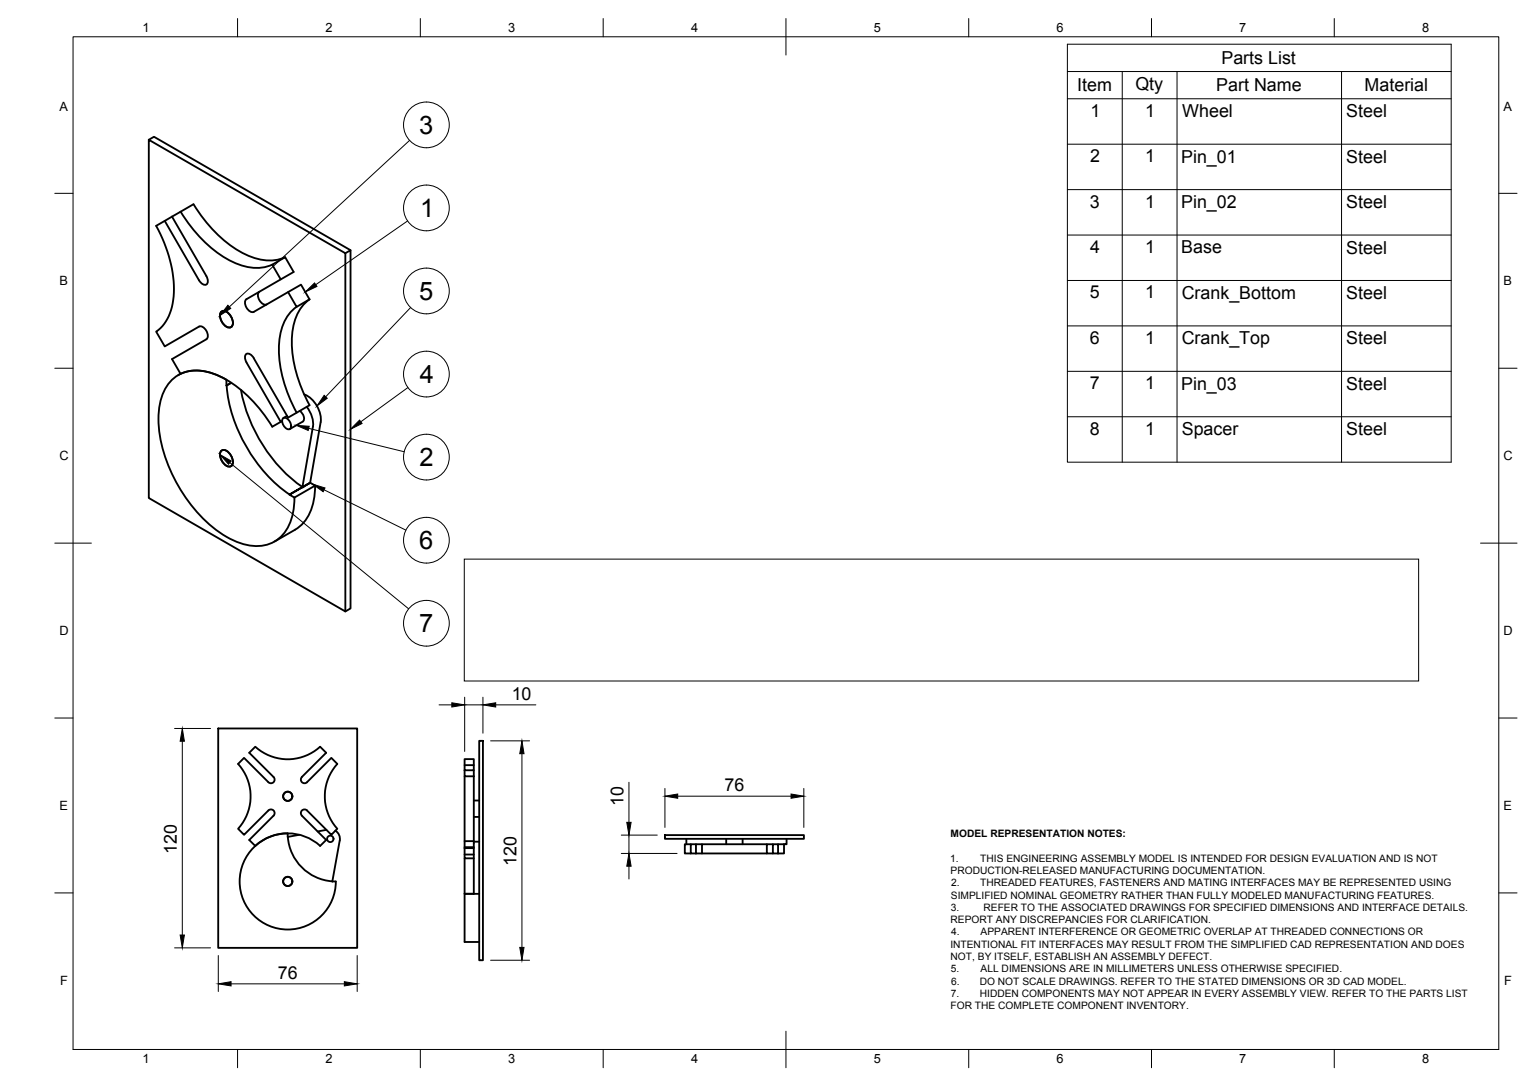
ISO-10303-21;
HEADER;
/* Generated by software containing ST-Developer
 * from STEP Tools, Inc. (www.steptools.com) 
 */

FILE_DESCRIPTION(
/* description */ (''),
/* implementation_level */ '2;1');

FILE_NAME(
/* name */ 'BR-051',
/* time_stamp */ '2026-09-20T21:52:48+06:00',
/* author */ (''),
/* organization */ (''),
/* preprocessor_version */ 'ST-DEVELOPER v20.2',
/* originating_system */ 'Autodesk Translation Framework v15.15.0.0',
/* authorisation */ '');

FILE_SCHEMA (('AUTOMOTIVE_DESIGN { 1 0 10303 214 3 1 1 }'));
ENDSEC;

DATA;
#10=MECHANICAL_DESIGN_GEOMETRIC_PRESENTATION_REPRESENTATION('',(#59,#60,
#61,#62,#63,#64,#65,#66),#2203);
#11=ITEM_DEFINED_TRANSFORMATION($,$,#1324,#1449);
#12=ITEM_DEFINED_TRANSFORMATION($,$,#1370,#1450);
#13=ITEM_DEFINED_TRANSFORMATION($,$,#1376,#1451);
#14=ITEM_DEFINED_TRANSFORMATION($,$,#1382,#1452);
#15=ITEM_DEFINED_TRANSFORMATION($,$,#1395,#1453);
#16=ITEM_DEFINED_TRANSFORMATION($,$,#1414,#1454);
#17=ITEM_DEFINED_TRANSFORMATION($,$,#1434,#1455);
#18=ITEM_DEFINED_TRANSFORMATION($,$,#1440,#1456);
#19=(
REPRESENTATION_RELATIONSHIP($,$,#2235,#2234)
REPRESENTATION_RELATIONSHIP_WITH_TRANSFORMATION(#11)
SHAPE_REPRESENTATION_RELATIONSHIP()
);
#20=(
REPRESENTATION_RELATIONSHIP($,$,#2236,#2234)
REPRESENTATION_RELATIONSHIP_WITH_TRANSFORMATION(#12)
SHAPE_REPRESENTATION_RELATIONSHIP()
);
#21=(
REPRESENTATION_RELATIONSHIP($,$,#2237,#2234)
REPRESENTATION_RELATIONSHIP_WITH_TRANSFORMATION(#13)
SHAPE_REPRESENTATION_RELATIONSHIP()
);
#22=(
REPRESENTATION_RELATIONSHIP($,$,#2238,#2234)
REPRESENTATION_RELATIONSHIP_WITH_TRANSFORMATION(#14)
SHAPE_REPRESENTATION_RELATIONSHIP()
);
#23=(
REPRESENTATION_RELATIONSHIP($,$,#2239,#2234)
REPRESENTATION_RELATIONSHIP_WITH_TRANSFORMATION(#15)
SHAPE_REPRESENTATION_RELATIONSHIP()
);
#24=(
REPRESENTATION_RELATIONSHIP($,$,#2240,#2234)
REPRESENTATION_RELATIONSHIP_WITH_TRANSFORMATION(#16)
SHAPE_REPRESENTATION_RELATIONSHIP()
);
#25=(
REPRESENTATION_RELATIONSHIP($,$,#2241,#2234)
REPRESENTATION_RELATIONSHIP_WITH_TRANSFORMATION(#17)
SHAPE_REPRESENTATION_RELATIONSHIP()
);
#26=(
REPRESENTATION_RELATIONSHIP($,$,#2242,#2234)
REPRESENTATION_RELATIONSHIP_WITH_TRANSFORMATION(#18)
SHAPE_REPRESENTATION_RELATIONSHIP()
);
#27=CONTEXT_DEPENDENT_SHAPE_REPRESENTATION(#19,#2226);
#28=CONTEXT_DEPENDENT_SHAPE_REPRESENTATION(#20,#2227);
#29=CONTEXT_DEPENDENT_SHAPE_REPRESENTATION(#21,#2228);
#30=CONTEXT_DEPENDENT_SHAPE_REPRESENTATION(#22,#2229);
#31=CONTEXT_DEPENDENT_SHAPE_REPRESENTATION(#23,#2230);
#32=CONTEXT_DEPENDENT_SHAPE_REPRESENTATION(#24,#2231);
#33=CONTEXT_DEPENDENT_SHAPE_REPRESENTATION(#25,#2232);
#34=CONTEXT_DEPENDENT_SHAPE_REPRESENTATION(#26,#2233);
#35=NEXT_ASSEMBLY_USAGE_OCCURRENCE('Wheel:1','Wheel:1','Wheel:1',#2244,
#2245,'Wheel:1');
#36=NEXT_ASSEMBLY_USAGE_OCCURRENCE('Pin_01:1','Pin_01:1','Pin_01:1',#2244,
#2246,'Pin_01:1');
#37=NEXT_ASSEMBLY_USAGE_OCCURRENCE('Pin_02:1','Pin_02:1','Pin_02:1',#2244,
#2247,'Pin_02:1');
#38=NEXT_ASSEMBLY_USAGE_OCCURRENCE('Base:1','Base:1','Base:1',#2244,#2248,
'Base:1');
#39=NEXT_ASSEMBLY_USAGE_OCCURRENCE('Crank_Bottom:1','Crank_Bottom:1',
'Crank_Bottom:1',#2244,#2249,'Crank_Bottom:1');
#40=NEXT_ASSEMBLY_USAGE_OCCURRENCE('Crank_Top:1','Crank_Top:1',
'Crank_Top:1',#2244,#2250,'Crank_Top:1');
#41=NEXT_ASSEMBLY_USAGE_OCCURRENCE('Pin_03:1','Pin_03:1','Pin_03:1',#2244,
#2251,'Pin_03:1');
#42=NEXT_ASSEMBLY_USAGE_OCCURRENCE('Spacer:1','Spacer:1','Spacer:1',#2244,
#2252,'Spacer:1');
#43=SHAPE_REPRESENTATION_RELATIONSHIP('SRR','None',#2235,#51);
#44=SHAPE_REPRESENTATION_RELATIONSHIP('SRR','None',#2236,#52);
#45=SHAPE_REPRESENTATION_RELATIONSHIP('SRR','None',#2237,#53);
#46=SHAPE_REPRESENTATION_RELATIONSHIP('SRR','None',#2238,#54);
#47=SHAPE_REPRESENTATION_RELATIONSHIP('SRR','None',#2239,#55);
#48=SHAPE_REPRESENTATION_RELATIONSHIP('SRR','None',#2240,#56);
#49=SHAPE_REPRESENTATION_RELATIONSHIP('SRR','None',#2241,#57);
#50=SHAPE_REPRESENTATION_RELATIONSHIP('SRR','None',#2242,#58);
#51=ADVANCED_BREP_SHAPE_REPRESENTATION('',(#67),#2195);
#52=ADVANCED_BREP_SHAPE_REPRESENTATION('',(#68),#2196);
#53=ADVANCED_BREP_SHAPE_REPRESENTATION('',(#69),#2197);
#54=ADVANCED_BREP_SHAPE_REPRESENTATION('',(#70),#2198);
#55=ADVANCED_BREP_SHAPE_REPRESENTATION('',(#71),#2199);
#56=ADVANCED_BREP_SHAPE_REPRESENTATION('',(#72),#2200);
#57=ADVANCED_BREP_SHAPE_REPRESENTATION('',(#73),#2201);
#58=ADVANCED_BREP_SHAPE_REPRESENTATION('',(#74),#2202);
#59=STYLED_ITEM('',(#2284),#67);
#60=STYLED_ITEM('',(#2285),#68);
#61=STYLED_ITEM('',(#2286),#69);
#62=STYLED_ITEM('',(#2286),#70);
#63=STYLED_ITEM('',(#2285),#71);
#64=STYLED_ITEM('',(#2285),#72);
#65=STYLED_ITEM('',(#2286),#73);
#66=STYLED_ITEM('',(#2286),#74);
#67=MANIFOLD_SOLID_BREP('Wheel',#1226);
#68=MANIFOLD_SOLID_BREP('Pin_01',#1227);
#69=MANIFOLD_SOLID_BREP('Pin_02',#1228);
#70=MANIFOLD_SOLID_BREP('Base',#1229);
#71=MANIFOLD_SOLID_BREP('Crank_Bottom',#1230);
#72=MANIFOLD_SOLID_BREP('Crank_Top',#1231);
#73=MANIFOLD_SOLID_BREP('Pin_03',#1232);
#74=MANIFOLD_SOLID_BREP('Spacer',#1233);
#75=FACE_BOUND('',#256,.T.);
#76=FACE_BOUND('',#258,.T.);
#77=FACE_BOUND('',#268,.T.);
#78=FACE_BOUND('',#269,.T.);
#79=FACE_BOUND('',#275,.T.);
#80=FACE_BOUND('',#276,.T.);
#81=FACE_BOUND('',#280,.T.);
#82=FACE_BOUND('',#281,.T.);
#83=FACE_BOUND('',#288,.T.);
#84=FACE_BOUND('',#289,.T.);
#85=FACE_BOUND('',#297,.T.);
#86=FACE_BOUND('',#303,.T.);
#87=FACE_BOUND('',#308,.T.);
#88=FACE_BOUND('',#312,.T.);
#89=CIRCLE('',#1327,2.);
#90=CIRCLE('',#1328,2.);
#91=CIRCLE('',#1334,2.);
#92=CIRCLE('',#1335,2.);
#93=CIRCLE('',#1339,26.3);
#94=CIRCLE('',#1340,26.3);
#95=CIRCLE('',#1344,2.);
#96=CIRCLE('',#1345,2.);
#97=CIRCLE('',#1349,26.3);
#98=CIRCLE('',#1350,26.3);
#99=CIRCLE('',#1354,2.);
#100=CIRCLE('',#1355,2.);
#101=CIRCLE('',#1359,26.3);
#102=CIRCLE('',#1360,26.3);
#103=CIRCLE('',#1362,2.5);
#104=CIRCLE('',#1363,2.5);
#105=CIRCLE('',#1365,26.3);
#106=CIRCLE('',#1366,26.3);
#107=CIRCLE('',#1372,1.75);
#108=CIRCLE('',#1374,1.75);
#109=CIRCLE('',#1378,2.5);
#110=CIRCLE('',#1380,2.5);
#111=CIRCLE('',#1384,2.5);
#112=CIRCLE('',#1385,2.5);
#113=CIRCLE('',#1387,2.5);
#114=CIRCLE('',#1388,2.5);
#115=CIRCLE('',#1399,5.25);
#116=CIRCLE('',#1400,24.399223777829);
#117=CIRCLE('',#1401,2.5);
#118=CIRCLE('',#1402,1.75);
#119=CIRCLE('',#1405,5.25);
#120=CIRCLE('',#1407,1.75);
#121=CIRCLE('',#1410,2.5);
#122=CIRCLE('',#1412,24.399223777829);
#123=CIRCLE('',#1417,24.399223777829);
#124=CIRCLE('',#1418,26.3);
#125=CIRCLE('',#1420,24.399223777829);
#126=CIRCLE('',#1422,26.3);
#127=CIRCLE('',#1425,26.3);
#128=CIRCLE('',#1426,2.5);
#129=CIRCLE('',#1428,26.3);
#130=CIRCLE('',#1430,2.5);
#131=CIRCLE('',#1436,2.5);
#132=CIRCLE('',#1438,2.5);
#133=CIRCLE('',#1442,4.5);
#134=CIRCLE('',#1443,2.5);
#135=CIRCLE('',#1445,4.5);
#136=CIRCLE('',#1447,2.5);
#137=CYLINDRICAL_SURFACE('',#1326,2.);
#138=CYLINDRICAL_SURFACE('',#1333,2.);
#139=CYLINDRICAL_SURFACE('',#1338,26.3);
#140=CYLINDRICAL_SURFACE('',#1343,2.);
#141=CYLINDRICAL_SURFACE('',#1348,26.3);
#142=CYLINDRICAL_SURFACE('',#1353,2.);
#143=CYLINDRICAL_SURFACE('',#1358,26.3);
#144=CYLINDRICAL_SURFACE('',#1361,2.5);
#145=CYLINDRICAL_SURFACE('',#1364,26.3);
#146=CYLINDRICAL_SURFACE('',#1373,1.75);
#147=CYLINDRICAL_SURFACE('',#1379,2.5);
#148=CYLINDRICAL_SURFACE('',#1383,2.5);
#149=CYLINDRICAL_SURFACE('',#1386,2.5);
#150=CYLINDRICAL_SURFACE('',#1404,5.25);
#151=CYLINDRICAL_SURFACE('',#1406,1.75);
#152=CYLINDRICAL_SURFACE('',#1409,2.5);
#153=CYLINDRICAL_SURFACE('',#1413,24.399223777829);
#154=CYLINDRICAL_SURFACE('',#1419,24.399223777829);
#155=CYLINDRICAL_SURFACE('',#1421,26.3);
#156=CYLINDRICAL_SURFACE('',#1427,26.3);
#157=CYLINDRICAL_SURFACE('',#1429,2.5);
#158=CYLINDRICAL_SURFACE('',#1437,2.5);
#159=CYLINDRICAL_SURFACE('',#1444,4.5);
#160=CYLINDRICAL_SURFACE('',#1446,2.5);
#161=FACE_OUTER_BOUND('',#230,.T.);
#162=FACE_OUTER_BOUND('',#231,.T.);
#163=FACE_OUTER_BOUND('',#232,.T.);
#164=FACE_OUTER_BOUND('',#233,.T.);
#165=FACE_OUTER_BOUND('',#234,.T.);
#166=FACE_OUTER_BOUND('',#235,.T.);
#167=FACE_OUTER_BOUND('',#236,.T.);
#168=FACE_OUTER_BOUND('',#237,.T.);
#169=FACE_OUTER_BOUND('',#238,.T.);
#170=FACE_OUTER_BOUND('',#239,.T.);
#171=FACE_OUTER_BOUND('',#240,.T.);
#172=FACE_OUTER_BOUND('',#241,.T.);
#173=FACE_OUTER_BOUND('',#242,.T.);
#174=FACE_OUTER_BOUND('',#243,.T.);
#175=FACE_OUTER_BOUND('',#244,.T.);
#176=FACE_OUTER_BOUND('',#245,.T.);
#177=FACE_OUTER_BOUND('',#246,.T.);
#178=FACE_OUTER_BOUND('',#247,.T.);
#179=FACE_OUTER_BOUND('',#248,.T.);
#180=FACE_OUTER_BOUND('',#249,.T.);
#181=FACE_OUTER_BOUND('',#250,.T.);
#182=FACE_OUTER_BOUND('',#251,.T.);
#183=FACE_OUTER_BOUND('',#252,.T.);
#184=FACE_OUTER_BOUND('',#253,.T.);
#185=FACE_OUTER_BOUND('',#254,.T.);
#186=FACE_OUTER_BOUND('',#255,.T.);
#187=FACE_OUTER_BOUND('',#257,.T.);
#188=FACE_OUTER_BOUND('',#259,.T.);
#189=FACE_OUTER_BOUND('',#260,.T.);
#190=FACE_OUTER_BOUND('',#261,.T.);
#191=FACE_OUTER_BOUND('',#262,.T.);
#192=FACE_OUTER_BOUND('',#263,.T.);
#193=FACE_OUTER_BOUND('',#264,.T.);
#194=FACE_OUTER_BOUND('',#265,.T.);
#195=FACE_OUTER_BOUND('',#266,.T.);
#196=FACE_OUTER_BOUND('',#267,.T.);
#197=FACE_OUTER_BOUND('',#270,.T.);
#198=FACE_OUTER_BOUND('',#271,.T.);
#199=FACE_OUTER_BOUND('',#272,.T.);
#200=FACE_OUTER_BOUND('',#273,.T.);
#201=FACE_OUTER_BOUND('',#274,.T.);
#202=FACE_OUTER_BOUND('',#277,.T.);
#203=FACE_OUTER_BOUND('',#278,.T.);
#204=FACE_OUTER_BOUND('',#279,.T.);
#205=FACE_OUTER_BOUND('',#282,.T.);
#206=FACE_OUTER_BOUND('',#283,.T.);
#207=FACE_OUTER_BOUND('',#284,.T.);
#208=FACE_OUTER_BOUND('',#285,.T.);
#209=FACE_OUTER_BOUND('',#286,.T.);
#210=FACE_OUTER_BOUND('',#287,.T.);
#211=FACE_OUTER_BOUND('',#290,.T.);
#212=FACE_OUTER_BOUND('',#291,.T.);
#213=FACE_OUTER_BOUND('',#292,.T.);
#214=FACE_OUTER_BOUND('',#293,.T.);
#215=FACE_OUTER_BOUND('',#294,.T.);
#216=FACE_OUTER_BOUND('',#295,.T.);
#217=FACE_OUTER_BOUND('',#296,.T.);
#218=FACE_OUTER_BOUND('',#298,.T.);
#219=FACE_OUTER_BOUND('',#299,.T.);
#220=FACE_OUTER_BOUND('',#300,.T.);
#221=FACE_OUTER_BOUND('',#301,.T.);
#222=FACE_OUTER_BOUND('',#302,.T.);
#223=FACE_OUTER_BOUND('',#304,.T.);
#224=FACE_OUTER_BOUND('',#305,.T.);
#225=FACE_OUTER_BOUND('',#306,.T.);
#226=FACE_OUTER_BOUND('',#307,.T.);
#227=FACE_OUTER_BOUND('',#309,.T.);
#228=FACE_OUTER_BOUND('',#310,.T.);
#229=FACE_OUTER_BOUND('',#311,.T.);
#230=EDGE_LOOP('',(#796,#797,#798,#799));
#231=EDGE_LOOP('',(#800,#801,#802,#803));
#232=EDGE_LOOP('',(#804,#805,#806,#807));
#233=EDGE_LOOP('',(#808,#809,#810,#811));
#234=EDGE_LOOP('',(#812,#813,#814,#815));
#235=EDGE_LOOP('',(#816,#817,#818,#819));
#236=EDGE_LOOP('',(#820,#821,#822,#823));
#237=EDGE_LOOP('',(#824,#825,#826,#827));
#238=EDGE_LOOP('',(#828,#829,#830,#831));
#239=EDGE_LOOP('',(#832,#833,#834,#835));
#240=EDGE_LOOP('',(#836,#837,#838,#839));
#241=EDGE_LOOP('',(#840,#841,#842,#843));
#242=EDGE_LOOP('',(#844,#845,#846,#847));
#243=EDGE_LOOP('',(#848,#849,#850,#851));
#244=EDGE_LOOP('',(#852,#853,#854,#855));
#245=EDGE_LOOP('',(#856,#857,#858,#859));
#246=EDGE_LOOP('',(#860,#861,#862,#863));
#247=EDGE_LOOP('',(#864,#865,#866,#867));
#248=EDGE_LOOP('',(#868,#869,#870,#871));
#249=EDGE_LOOP('',(#872,#873,#874,#875));
#250=EDGE_LOOP('',(#876,#877,#878,#879));
#251=EDGE_LOOP('',(#880,#881,#882,#883));
#252=EDGE_LOOP('',(#884,#885,#886,#887));
#253=EDGE_LOOP('',(#888,#889,#890,#891));
#254=EDGE_LOOP('',(#892,#893,#894,#895));
#255=EDGE_LOOP('',(#896,#897,#898,#899,#900,#901,#902,#903,#904,#905,#906,
#907,#908,#909,#910,#911,#912,#913,#914,#915,#916,#917,#918,#919));
#256=EDGE_LOOP('',(#920));
#257=EDGE_LOOP('',(#921,#922,#923,#924,#925,#926,#927,#928,#929,#930,#931,
#932,#933,#934,#935,#936,#937,#938,#939,#940,#941,#942,#943,#944));
#258=EDGE_LOOP('',(#945));
#259=EDGE_LOOP('',(#946));
#260=EDGE_LOOP('',(#947,#948,#949,#950));
#261=EDGE_LOOP('',(#951));
#262=EDGE_LOOP('',(#952));
#263=EDGE_LOOP('',(#953,#954,#955,#956));
#264=EDGE_LOOP('',(#957));
#265=EDGE_LOOP('',(#958,#959,#960,#961));
#266=EDGE_LOOP('',(#962,#963,#964,#965));
#267=EDGE_LOOP('',(#966,#967,#968,#969));
#268=EDGE_LOOP('',(#970));
#269=EDGE_LOOP('',(#971));
#270=EDGE_LOOP('',(#972,#973,#974,#975));
#271=EDGE_LOOP('',(#976,#977,#978,#979));
#272=EDGE_LOOP('',(#980,#981,#982,#983));
#273=EDGE_LOOP('',(#984,#985,#986,#987));
#274=EDGE_LOOP('',(#988,#989,#990,#991));
#275=EDGE_LOOP('',(#992));
#276=EDGE_LOOP('',(#993));
#277=EDGE_LOOP('',(#994,#995,#996,#997));
#278=EDGE_LOOP('',(#998,#999,#1000,#1001));
#279=EDGE_LOOP('',(#1002,#1003,#1004,#1005,#1006,#1007));
#280=EDGE_LOOP('',(#1008));
#281=EDGE_LOOP('',(#1009));
#282=EDGE_LOOP('',(#1010,#1011,#1012,#1013));
#283=EDGE_LOOP('',(#1014,#1015,#1016,#1017));
#284=EDGE_LOOP('',(#1018,#1019,#1020,#1021));
#285=EDGE_LOOP('',(#1022,#1023,#1024,#1025));
#286=EDGE_LOOP('',(#1026,#1027,#1028,#1029));
#287=EDGE_LOOP('',(#1030,#1031,#1032,#1033,#1034,#1035));
#288=EDGE_LOOP('',(#1036));
#289=EDGE_LOOP('',(#1037));
#290=EDGE_LOOP('',(#1038,#1039,#1040,#1041));
#291=EDGE_LOOP('',(#1042,#1043,#1044,#1045,#1046));
#292=EDGE_LOOP('',(#1047,#1048,#1049,#1050));
#293=EDGE_LOOP('',(#1051,#1052,#1053,#1054));
#294=EDGE_LOOP('',(#1055,#1056,#1057,#1058));
#295=EDGE_LOOP('',(#1059,#1060,#1061,#1062));
#296=EDGE_LOOP('',(#1063,#1064,#1065,#1066,#1067,#1068));
#297=EDGE_LOOP('',(#1069));
#298=EDGE_LOOP('',(#1070,#1071,#1072,#1073));
#299=EDGE_LOOP('',(#1074,#1075,#1076,#1077));
#300=EDGE_LOOP('',(#1078,#1079,#1080,#1081,#1082,#1083));
#301=EDGE_LOOP('',(#1084,#1085,#1086,#1087));
#302=EDGE_LOOP('',(#1088,#1089,#1090,#1091,#1092));
#303=EDGE_LOOP('',(#1093));
#304=EDGE_LOOP('',(#1094));
#305=EDGE_LOOP('',(#1095,#1096,#1097,#1098));
#306=EDGE_LOOP('',(#1099));
#307=EDGE_LOOP('',(#1100));
#308=EDGE_LOOP('',(#1101));
#309=EDGE_LOOP('',(#1102,#1103,#1104,#1105));
#310=EDGE_LOOP('',(#1106,#1107,#1108,#1109));
#311=EDGE_LOOP('',(#1110));
#312=EDGE_LOOP('',(#1111));
#313=LINE('',#1840,#423);
#314=LINE('',#1842,#424);
#315=LINE('',#1844,#425);
#316=LINE('',#1845,#426);
#317=LINE('',#1851,#427);
#318=LINE('',#1854,#428);
#319=LINE('',#1856,#429);
#320=LINE('',#1857,#430);
#321=LINE('',#1860,#431);
#322=LINE('',#1862,#432);
#323=LINE('',#1863,#433);
#324=LINE('',#1866,#434);
#325=LINE('',#1868,#435);
#326=LINE('',#1869,#436);
#327=LINE('',#1873,#437);
#328=LINE('',#1875,#438);
#329=LINE('',#1877,#439);
#330=LINE('',#1878,#440);
#331=LINE('',#1883,#441);
#332=LINE('',#1887,#442);
#333=LINE('',#1889,#443);
#334=LINE('',#1890,#444);
#335=LINE('',#1893,#445);
#336=LINE('',#1895,#446);
#337=LINE('',#1896,#447);
#338=LINE('',#1902,#448);
#339=LINE('',#1904,#449);
#340=LINE('',#1905,#450);
#341=LINE('',#1909,#451);
#342=LINE('',#1911,#452);
#343=LINE('',#1913,#453);
#344=LINE('',#1914,#454);
#345=LINE('',#1919,#455);
#346=LINE('',#1923,#456);
#347=LINE('',#1925,#457);
#348=LINE('',#1926,#458);
#349=LINE('',#1929,#459);
#350=LINE('',#1931,#460);
#351=LINE('',#1932,#461);
#352=LINE('',#1937,#462);
#353=LINE('',#1940,#463);
#354=LINE('',#1941,#464);
#355=LINE('',#1945,#465);
#356=LINE('',#1947,#466);
#357=LINE('',#1949,#467);
#358=LINE('',#1950,#468);
#359=LINE('',#1956,#469);
#360=LINE('',#1959,#470);
#361=LINE('',#1961,#471);
#362=LINE('',#1962,#472);
#363=LINE('',#1965,#473);
#364=LINE('',#1967,#474);
#365=LINE('',#1968,#475);
#366=LINE('',#1976,#476);
#367=LINE('',#1983,#477);
#368=LINE('',#1985,#478);
#369=LINE('',#1986,#479);
#370=LINE('',#1995,#480);
#371=LINE('',#2004,#481);
#372=LINE('',#2012,#482);
#373=LINE('',#2018,#483);
#374=LINE('',#2023,#484);
#375=LINE('',#2025,#485);
#376=LINE('',#2027,#486);
#377=LINE('',#2028,#487);
#378=LINE('',#2031,#488);
#379=LINE('',#2033,#489);
#380=LINE('',#2034,#490);
#381=LINE('',#2037,#491);
#382=LINE('',#2038,#492);
#383=LINE('',#2041,#493);
#384=LINE('',#2042,#494);
#385=LINE('',#2044,#495);
#386=LINE('',#2050,#496);
#387=LINE('',#2052,#497);
#388=LINE('',#2054,#498);
#389=LINE('',#2055,#499);
#390=LINE('',#2059,#500);
#391=LINE('',#2061,#501);
#392=LINE('',#2063,#502);
#393=LINE('',#2064,#503);
#394=LINE('',#2067,#504);
#395=LINE('',#2070,#505);
#396=LINE('',#2078,#506);
#397=LINE('',#2079,#507);
#398=LINE('',#2084,#508);
#399=LINE('',#2088,#509);
#400=LINE('',#2089,#510);
#401=LINE('',#2092,#511);
#402=LINE('',#2101,#512);
#403=LINE('',#2103,#513);
#404=LINE('',#2105,#514);
#405=LINE('',#2107,#515);
#406=LINE('',#2108,#516);
#407=LINE('',#2113,#517);
#408=LINE('',#2118,#518);
#409=LINE('',#2121,#519);
#410=LINE('',#2126,#520);
#411=LINE('',#2128,#521);
#412=LINE('',#2130,#522);
#413=LINE('',#2131,#523);
#414=LINE('',#2134,#524);
#415=LINE('',#2135,#525);
#416=LINE('',#2141,#526);
#417=LINE('',#2146,#527);
#418=LINE('',#2148,#528);
#419=LINE('',#2150,#529);
#420=LINE('',#2158,#530);
#421=LINE('',#2169,#531);
#422=LINE('',#2174,#532);
#423=VECTOR('',#1463,10.);
#424=VECTOR('',#1464,10.);
#425=VECTOR('',#1465,10.);
#426=VECTOR('',#1466,10.);
#427=VECTOR('',#1473,10.);
#428=VECTOR('',#1476,10.);
#429=VECTOR('',#1477,10.);
#430=VECTOR('',#1478,10.);
#431=VECTOR('',#1481,10.);
#432=VECTOR('',#1482,10.);
#433=VECTOR('',#1483,10.);
#434=VECTOR('',#1486,10.);
#435=VECTOR('',#1487,10.);
#436=VECTOR('',#1488,10.);
#437=VECTOR('',#1491,10.);
#438=VECTOR('',#1492,10.);
#439=VECTOR('',#1493,10.);
#440=VECTOR('',#1494,10.);
#441=VECTOR('',#1499,10.);
#442=VECTOR('',#1504,10.);
#443=VECTOR('',#1505,10.);
#444=VECTOR('',#1506,10.);
#445=VECTOR('',#1509,10.);
#446=VECTOR('',#1510,10.);
#447=VECTOR('',#1511,10.);
#448=VECTOR('',#1520,10.);
#449=VECTOR('',#1521,10.);
#450=VECTOR('',#1522,10.);
#451=VECTOR('',#1525,10.);
#452=VECTOR('',#1526,10.);
#453=VECTOR('',#1527,10.);
#454=VECTOR('',#1528,10.);
#455=VECTOR('',#1533,10.);
#456=VECTOR('',#1538,10.);
#457=VECTOR('',#1539,10.);
#458=VECTOR('',#1540,10.);
#459=VECTOR('',#1543,10.);
#460=VECTOR('',#1544,10.);
#461=VECTOR('',#1545,10.);
#462=VECTOR('',#1550,10.);
#463=VECTOR('',#1555,10.);
#464=VECTOR('',#1556,10.);
#465=VECTOR('',#1559,10.);
#466=VECTOR('',#1560,10.);
#467=VECTOR('',#1561,10.);
#468=VECTOR('',#1562,10.);
#469=VECTOR('',#1569,10.);
#470=VECTOR('',#1572,10.);
#471=VECTOR('',#1573,10.);
#472=VECTOR('',#1574,10.);
#473=VECTOR('',#1577,10.);
#474=VECTOR('',#1578,10.);
#475=VECTOR('',#1579,10.);
#476=VECTOR('',#1590,2.5);
#477=VECTOR('',#1599,10.);
#478=VECTOR('',#1602,10.);
#479=VECTOR('',#1603,10.);
#480=VECTOR('',#1616,1.75);
#481=VECTOR('',#1629,2.5);
#482=VECTOR('',#1640,2.5);
#483=VECTOR('',#1647,2.5);
#484=VECTOR('',#1652,10.);
#485=VECTOR('',#1653,10.);
#486=VECTOR('',#1654,10.);
#487=VECTOR('',#1655,10.);
#488=VECTOR('',#1658,10.);
#489=VECTOR('',#1659,10.);
#490=VECTOR('',#1660,10.);
#491=VECTOR('',#1663,10.);
#492=VECTOR('',#1664,10.);
#493=VECTOR('',#1667,10.);
#494=VECTOR('',#1668,10.);
#495=VECTOR('',#1671,10.);
#496=VECTOR('',#1678,10.);
#497=VECTOR('',#1679,10.);
#498=VECTOR('',#1680,10.);
#499=VECTOR('',#1681,10.);
#500=VECTOR('',#1684,10.);
#501=VECTOR('',#1685,10.);
#502=VECTOR('',#1686,10.);
#503=VECTOR('',#1687,10.);
#504=VECTOR('',#1690,10.);
#505=VECTOR('',#1693,10.);
#506=VECTOR('',#1702,10.);
#507=VECTOR('',#1703,10.);
#508=VECTOR('',#1710,1.75);
#509=VECTOR('',#1715,10.);
#510=VECTOR('',#1716,10.);
#511=VECTOR('',#1719,2.5);
#512=VECTOR('',#1732,10.);
#513=VECTOR('',#1733,10.);
#514=VECTOR('',#1734,10.);
#515=VECTOR('',#1735,10.);
#516=VECTOR('',#1736,10.);
#517=VECTOR('',#1741,10.);
#518=VECTOR('',#1748,10.);
#519=VECTOR('',#1751,10.);
#520=VECTOR('',#1756,10.);
#521=VECTOR('',#1757,10.);
#522=VECTOR('',#1758,10.);
#523=VECTOR('',#1759,10.);
#524=VECTOR('',#1762,10.);
#525=VECTOR('',#1763,10.);
#526=VECTOR('',#1770,10.);
#527=VECTOR('',#1777,2.5);
#528=VECTOR('',#1780,10.);
#529=VECTOR('',#1783,10.);
#530=VECTOR('',#1794,2.5);
#531=VECTOR('',#1809,4.5);
#532=VECTOR('',#1816,2.5);
#533=VERTEX_POINT('',#1838);
#534=VERTEX_POINT('',#1839);
#535=VERTEX_POINT('',#1841);
#536=VERTEX_POINT('',#1843);
#537=VERTEX_POINT('',#1847);
#538=VERTEX_POINT('',#1849);
#539=VERTEX_POINT('',#1853);
#540=VERTEX_POINT('',#1855);
#541=VERTEX_POINT('',#1859);
#542=VERTEX_POINT('',#1861);
#543=VERTEX_POINT('',#1865);
#544=VERTEX_POINT('',#1867);
#545=VERTEX_POINT('',#1871);
#546=VERTEX_POINT('',#1872);
#547=VERTEX_POINT('',#1874);
#548=VERTEX_POINT('',#1876);
#549=VERTEX_POINT('',#1880);
#550=VERTEX_POINT('',#1882);
#551=VERTEX_POINT('',#1886);
#552=VERTEX_POINT('',#1888);
#553=VERTEX_POINT('',#1892);
#554=VERTEX_POINT('',#1894);
#555=VERTEX_POINT('',#1901);
#556=VERTEX_POINT('',#1903);
#557=VERTEX_POINT('',#1907);
#558=VERTEX_POINT('',#1908);
#559=VERTEX_POINT('',#1910);
#560=VERTEX_POINT('',#1912);
#561=VERTEX_POINT('',#1916);
#562=VERTEX_POINT('',#1918);
#563=VERTEX_POINT('',#1922);
#564=VERTEX_POINT('',#1924);
#565=VERTEX_POINT('',#1928);
#566=VERTEX_POINT('',#1930);
#567=VERTEX_POINT('',#1934);
#568=VERTEX_POINT('',#1936);
#569=VERTEX_POINT('',#1943);
#570=VERTEX_POINT('',#1944);
#571=VERTEX_POINT('',#1946);
#572=VERTEX_POINT('',#1948);
#573=VERTEX_POINT('',#1952);
#574=VERTEX_POINT('',#1954);
#575=VERTEX_POINT('',#1958);
#576=VERTEX_POINT('',#1960);
#577=VERTEX_POINT('',#1964);
#578=VERTEX_POINT('',#1966);
#579=VERTEX_POINT('',#1973);
#580=VERTEX_POINT('',#1975);
#581=VERTEX_POINT('',#1979);
#582=VERTEX_POINT('',#1981);
#583=VERTEX_POINT('',#1991);
#584=VERTEX_POINT('',#1994);
#585=VERTEX_POINT('',#2000);
#586=VERTEX_POINT('',#2003);
#587=VERTEX_POINT('',#2009);
#588=VERTEX_POINT('',#2011);
#589=VERTEX_POINT('',#2015);
#590=VERTEX_POINT('',#2017);
#591=VERTEX_POINT('',#2021);
#592=VERTEX_POINT('',#2022);
#593=VERTEX_POINT('',#2024);
#594=VERTEX_POINT('',#2026);
#595=VERTEX_POINT('',#2030);
#596=VERTEX_POINT('',#2032);
#597=VERTEX_POINT('',#2036);
#598=VERTEX_POINT('',#2040);
#599=VERTEX_POINT('',#2048);
#600=VERTEX_POINT('',#2049);
#601=VERTEX_POINT('',#2051);
#602=VERTEX_POINT('',#2053);
#603=VERTEX_POINT('',#2057);
#604=VERTEX_POINT('',#2058);
#605=VERTEX_POINT('',#2060);
#606=VERTEX_POINT('',#2062);
#607=VERTEX_POINT('',#2066);
#608=VERTEX_POINT('',#2069);
#609=VERTEX_POINT('',#2072);
#610=VERTEX_POINT('',#2074);
#611=VERTEX_POINT('',#2077);
#612=VERTEX_POINT('',#2083);
#613=VERTEX_POINT('',#2087);
#614=VERTEX_POINT('',#2091);
#615=VERTEX_POINT('',#2099);
#616=VERTEX_POINT('',#2100);
#617=VERTEX_POINT('',#2102);
#618=VERTEX_POINT('',#2104);
#619=VERTEX_POINT('',#2106);
#620=VERTEX_POINT('',#2110);
#621=VERTEX_POINT('',#2112);
#622=VERTEX_POINT('',#2116);
#623=VERTEX_POINT('',#2120);
#624=VERTEX_POINT('',#2124);
#625=VERTEX_POINT('',#2125);
#626=VERTEX_POINT('',#2127);
#627=VERTEX_POINT('',#2129);
#628=VERTEX_POINT('',#2133);
#629=VERTEX_POINT('',#2137);
#630=VERTEX_POINT('',#2140);
#631=VERTEX_POINT('',#2144);
#632=VERTEX_POINT('',#2154);
#633=VERTEX_POINT('',#2157);
#634=VERTEX_POINT('',#2163);
#635=VERTEX_POINT('',#2165);
#636=VERTEX_POINT('',#2168);
#637=VERTEX_POINT('',#2172);
#638=EDGE_CURVE('',#533,#534,#313,.T.);
#639=EDGE_CURVE('',#534,#535,#314,.T.);
#640=EDGE_CURVE('',#536,#535,#315,.T.);
#641=EDGE_CURVE('',#533,#536,#316,.T.);
#642=EDGE_CURVE('',#537,#533,#89,.T.);
#643=EDGE_CURVE('',#538,#536,#90,.T.);
#644=EDGE_CURVE('',#537,#538,#317,.T.);
#645=EDGE_CURVE('',#539,#537,#318,.T.);
#646=EDGE_CURVE('',#540,#538,#319,.T.);
#647=EDGE_CURVE('',#539,#540,#320,.T.);
#648=EDGE_CURVE('',#539,#541,#321,.T.);
#649=EDGE_CURVE('',#542,#540,#322,.T.);
#650=EDGE_CURVE('',#541,#542,#323,.T.);
#651=EDGE_CURVE('',#543,#534,#324,.T.);
#652=EDGE_CURVE('',#543,#544,#325,.T.);
#653=EDGE_CURVE('',#535,#544,#326,.T.);
#654=EDGE_CURVE('',#545,#546,#327,.T.);
#655=EDGE_CURVE('',#545,#547,#328,.T.);
#656=EDGE_CURVE('',#547,#548,#329,.T.);
#657=EDGE_CURVE('',#546,#548,#330,.T.);
#658=EDGE_CURVE('',#549,#545,#91,.T.);
#659=EDGE_CURVE('',#549,#550,#331,.T.);
#660=EDGE_CURVE('',#550,#547,#92,.T.);
#661=EDGE_CURVE('',#551,#549,#332,.T.);
#662=EDGE_CURVE('',#551,#552,#333,.T.);
#663=EDGE_CURVE('',#552,#550,#334,.T.);
#664=EDGE_CURVE('',#551,#553,#335,.T.);
#665=EDGE_CURVE('',#553,#554,#336,.T.);
#666=EDGE_CURVE('',#554,#552,#337,.T.);
#667=EDGE_CURVE('',#541,#553,#93,.T.);
#668=EDGE_CURVE('',#554,#542,#94,.T.);
#669=EDGE_CURVE('',#555,#546,#338,.T.);
#670=EDGE_CURVE('',#548,#556,#339,.T.);
#671=EDGE_CURVE('',#555,#556,#340,.T.);
#672=EDGE_CURVE('',#557,#558,#341,.T.);
#673=EDGE_CURVE('',#557,#559,#342,.T.);
#674=EDGE_CURVE('',#559,#560,#343,.T.);
#675=EDGE_CURVE('',#558,#560,#344,.T.);
#676=EDGE_CURVE('',#561,#557,#95,.T.);
#677=EDGE_CURVE('',#561,#562,#345,.T.);
#678=EDGE_CURVE('',#562,#559,#96,.T.);
#679=EDGE_CURVE('',#563,#561,#346,.T.);
#680=EDGE_CURVE('',#563,#564,#347,.T.);
#681=EDGE_CURVE('',#564,#562,#348,.T.);
#682=EDGE_CURVE('',#563,#565,#349,.T.);
#683=EDGE_CURVE('',#565,#566,#350,.T.);
#684=EDGE_CURVE('',#566,#564,#351,.T.);
#685=EDGE_CURVE('',#543,#567,#97,.T.);
#686=EDGE_CURVE('',#567,#568,#352,.T.);
#687=EDGE_CURVE('',#544,#568,#98,.T.);
#688=EDGE_CURVE('',#567,#558,#353,.T.);
#689=EDGE_CURVE('',#560,#568,#354,.T.);
#690=EDGE_CURVE('',#569,#570,#355,.T.);
#691=EDGE_CURVE('',#570,#571,#356,.T.);
#692=EDGE_CURVE('',#572,#571,#357,.T.);
#693=EDGE_CURVE('',#569,#572,#358,.T.);
#694=EDGE_CURVE('',#573,#569,#99,.T.);
#695=EDGE_CURVE('',#574,#572,#100,.T.);
#696=EDGE_CURVE('',#573,#574,#359,.T.);
#697=EDGE_CURVE('',#575,#573,#360,.T.);
#698=EDGE_CURVE('',#576,#574,#361,.T.);
#699=EDGE_CURVE('',#575,#576,#362,.T.);
#700=EDGE_CURVE('',#575,#577,#363,.T.);
#701=EDGE_CURVE('',#578,#576,#364,.T.);
#702=EDGE_CURVE('',#577,#578,#365,.T.);
#703=EDGE_CURVE('',#565,#577,#101,.T.);
#704=EDGE_CURVE('',#578,#566,#102,.T.);
#705=EDGE_CURVE('',#579,#579,#103,.T.);
#706=EDGE_CURVE('',#579,#580,#366,.T.);
#707=EDGE_CURVE('',#580,#580,#104,.T.);
#708=EDGE_CURVE('',#581,#555,#105,.T.);
#709=EDGE_CURVE('',#582,#556,#106,.T.);
#710=EDGE_CURVE('',#581,#582,#367,.T.);
#711=EDGE_CURVE('',#581,#570,#368,.T.);
#712=EDGE_CURVE('',#571,#582,#369,.T.);
#713=EDGE_CURVE('',#583,#583,#107,.T.);
#714=EDGE_CURVE('',#583,#584,#370,.T.);
#715=EDGE_CURVE('',#584,#584,#108,.T.);
#716=EDGE_CURVE('',#585,#585,#109,.T.);
#717=EDGE_CURVE('',#585,#586,#371,.T.);
#718=EDGE_CURVE('',#586,#586,#110,.T.);
#719=EDGE_CURVE('',#587,#587,#111,.T.);
#720=EDGE_CURVE('',#587,#588,#372,.T.);
#721=EDGE_CURVE('',#588,#588,#112,.T.);
#722=EDGE_CURVE('',#589,#589,#113,.T.);
#723=EDGE_CURVE('',#589,#590,#373,.T.);
#724=EDGE_CURVE('',#590,#590,#114,.T.);
#725=EDGE_CURVE('',#591,#592,#374,.T.);
#726=EDGE_CURVE('',#593,#591,#375,.T.);
#727=EDGE_CURVE('',#594,#593,#376,.T.);
#728=EDGE_CURVE('',#592,#594,#377,.T.);
#729=EDGE_CURVE('',#591,#595,#378,.T.);
#730=EDGE_CURVE('',#596,#595,#379,.T.);
#731=EDGE_CURVE('',#593,#596,#380,.T.);
#732=EDGE_CURVE('',#592,#597,#381,.T.);
#733=EDGE_CURVE('',#595,#597,#382,.T.);
#734=EDGE_CURVE('',#598,#596,#383,.T.);
#735=EDGE_CURVE('',#594,#598,#384,.T.);
#736=EDGE_CURVE('',#597,#598,#385,.T.);
#737=EDGE_CURVE('',#599,#600,#386,.T.);
#738=EDGE_CURVE('',#600,#601,#387,.T.);
#739=EDGE_CURVE('',#602,#601,#388,.T.);
#740=EDGE_CURVE('',#599,#602,#389,.T.);
#741=EDGE_CURVE('',#603,#604,#390,.T.);
#742=EDGE_CURVE('',#604,#605,#391,.T.);
#743=EDGE_CURVE('',#606,#605,#392,.T.);
#744=EDGE_CURVE('',#603,#606,#393,.T.);
#745=EDGE_CURVE('',#605,#607,#394,.T.);
#746=EDGE_CURVE('',#607,#602,#115,.T.);
#747=EDGE_CURVE('',#601,#608,#395,.T.);
#748=EDGE_CURVE('',#606,#608,#116,.T.);
#749=EDGE_CURVE('',#609,#609,#117,.T.);
#750=EDGE_CURVE('',#610,#610,#118,.T.);
#751=EDGE_CURVE('',#604,#611,#396,.T.);
#752=EDGE_CURVE('',#611,#607,#397,.T.);
#753=EDGE_CURVE('',#611,#599,#119,.T.);
#754=EDGE_CURVE('',#610,#612,#398,.T.);
#755=EDGE_CURVE('',#612,#612,#120,.T.);
#756=EDGE_CURVE('',#600,#613,#399,.T.);
#757=EDGE_CURVE('',#608,#613,#400,.T.);
#758=EDGE_CURVE('',#609,#614,#401,.T.);
#759=EDGE_CURVE('',#614,#614,#121,.T.);
#760=EDGE_CURVE('',#613,#603,#122,.T.);
#761=EDGE_CURVE('',#615,#616,#402,.T.);
#762=EDGE_CURVE('',#617,#615,#403,.T.);
#763=EDGE_CURVE('',#618,#617,#404,.T.);
#764=EDGE_CURVE('',#619,#618,#405,.T.);
#765=EDGE_CURVE('',#619,#616,#406,.T.);
#766=EDGE_CURVE('',#615,#620,#123,.T.);
#767=EDGE_CURVE('',#620,#621,#407,.T.);
#768=EDGE_CURVE('',#621,#617,#124,.T.);
#769=EDGE_CURVE('',#622,#616,#125,.T.);
#770=EDGE_CURVE('',#620,#622,#408,.T.);
#771=EDGE_CURVE('',#621,#623,#409,.T.);
#772=EDGE_CURVE('',#618,#623,#126,.T.);
#773=EDGE_CURVE('',#624,#625,#410,.T.);
#774=EDGE_CURVE('',#626,#624,#411,.T.);
#775=EDGE_CURVE('',#627,#626,#412,.T.);
#776=EDGE_CURVE('',#627,#625,#413,.T.);
#777=EDGE_CURVE('',#628,#619,#414,.T.);
#778=EDGE_CURVE('',#623,#627,#415,.T.);
#779=EDGE_CURVE('',#626,#628,#127,.T.);
#780=EDGE_CURVE('',#629,#629,#128,.T.);
#781=EDGE_CURVE('',#630,#628,#416,.T.);
#782=EDGE_CURVE('',#624,#630,#129,.T.);
#783=EDGE_CURVE('',#631,#631,#130,.T.);
#784=EDGE_CURVE('',#631,#629,#417,.T.);
#785=EDGE_CURVE('',#625,#622,#418,.T.);
#786=EDGE_CURVE('',#616,#630,#419,.T.);
#787=EDGE_CURVE('',#632,#632,#131,.T.);
#788=EDGE_CURVE('',#632,#633,#420,.T.);
#789=EDGE_CURVE('',#633,#633,#132,.T.);
#790=EDGE_CURVE('',#634,#634,#133,.T.);
#791=EDGE_CURVE('',#635,#635,#134,.T.);
#792=EDGE_CURVE('',#634,#636,#421,.T.);
#793=EDGE_CURVE('',#636,#636,#135,.T.);
#794=EDGE_CURVE('',#637,#637,#136,.T.);
#795=EDGE_CURVE('',#637,#635,#422,.T.);
#796=ORIENTED_EDGE('',*,*,#638,.T.);
#797=ORIENTED_EDGE('',*,*,#639,.T.);
#798=ORIENTED_EDGE('',*,*,#640,.F.);
#799=ORIENTED_EDGE('',*,*,#641,.F.);
#800=ORIENTED_EDGE('',*,*,#642,.T.);
#801=ORIENTED_EDGE('',*,*,#641,.T.);
#802=ORIENTED_EDGE('',*,*,#643,.F.);
#803=ORIENTED_EDGE('',*,*,#644,.F.);
#804=ORIENTED_EDGE('',*,*,#645,.T.);
#805=ORIENTED_EDGE('',*,*,#644,.T.);
#806=ORIENTED_EDGE('',*,*,#646,.F.);
#807=ORIENTED_EDGE('',*,*,#647,.F.);
#808=ORIENTED_EDGE('',*,*,#648,.F.);
#809=ORIENTED_EDGE('',*,*,#647,.T.);
#810=ORIENTED_EDGE('',*,*,#649,.F.);
#811=ORIENTED_EDGE('',*,*,#650,.F.);
#812=ORIENTED_EDGE('',*,*,#651,.F.);
#813=ORIENTED_EDGE('',*,*,#652,.T.);
#814=ORIENTED_EDGE('',*,*,#653,.F.);
#815=ORIENTED_EDGE('',*,*,#639,.F.);
#816=ORIENTED_EDGE('',*,*,#654,.F.);
#817=ORIENTED_EDGE('',*,*,#655,.T.);
#818=ORIENTED_EDGE('',*,*,#656,.T.);
#819=ORIENTED_EDGE('',*,*,#657,.F.);
#820=ORIENTED_EDGE('',*,*,#658,.F.);
#821=ORIENTED_EDGE('',*,*,#659,.T.);
#822=ORIENTED_EDGE('',*,*,#660,.T.);
#823=ORIENTED_EDGE('',*,*,#655,.F.);
#824=ORIENTED_EDGE('',*,*,#661,.F.);
#825=ORIENTED_EDGE('',*,*,#662,.T.);
#826=ORIENTED_EDGE('',*,*,#663,.T.);
#827=ORIENTED_EDGE('',*,*,#659,.F.);
#828=ORIENTED_EDGE('',*,*,#664,.T.);
#829=ORIENTED_EDGE('',*,*,#665,.T.);
#830=ORIENTED_EDGE('',*,*,#666,.T.);
#831=ORIENTED_EDGE('',*,*,#662,.F.);
#832=ORIENTED_EDGE('',*,*,#667,.F.);
#833=ORIENTED_EDGE('',*,*,#650,.T.);
#834=ORIENTED_EDGE('',*,*,#668,.F.);
#835=ORIENTED_EDGE('',*,*,#665,.F.);
#836=ORIENTED_EDGE('',*,*,#669,.T.);
#837=ORIENTED_EDGE('',*,*,#657,.T.);
#838=ORIENTED_EDGE('',*,*,#670,.T.);
#839=ORIENTED_EDGE('',*,*,#671,.F.);
#840=ORIENTED_EDGE('',*,*,#672,.F.);
#841=ORIENTED_EDGE('',*,*,#673,.T.);
#842=ORIENTED_EDGE('',*,*,#674,.T.);
#843=ORIENTED_EDGE('',*,*,#675,.F.);
#844=ORIENTED_EDGE('',*,*,#676,.F.);
#845=ORIENTED_EDGE('',*,*,#677,.T.);
#846=ORIENTED_EDGE('',*,*,#678,.T.);
#847=ORIENTED_EDGE('',*,*,#673,.F.);
#848=ORIENTED_EDGE('',*,*,#679,.F.);
#849=ORIENTED_EDGE('',*,*,#680,.T.);
#850=ORIENTED_EDGE('',*,*,#681,.T.);
#851=ORIENTED_EDGE('',*,*,#677,.F.);
#852=ORIENTED_EDGE('',*,*,#682,.T.);
#853=ORIENTED_EDGE('',*,*,#683,.T.);
#854=ORIENTED_EDGE('',*,*,#684,.T.);
#855=ORIENTED_EDGE('',*,*,#680,.F.);
#856=ORIENTED_EDGE('',*,*,#685,.T.);
#857=ORIENTED_EDGE('',*,*,#686,.T.);
#858=ORIENTED_EDGE('',*,*,#687,.F.);
#859=ORIENTED_EDGE('',*,*,#652,.F.);
#860=ORIENTED_EDGE('',*,*,#688,.T.);
#861=ORIENTED_EDGE('',*,*,#675,.T.);
#862=ORIENTED_EDGE('',*,*,#689,.T.);
#863=ORIENTED_EDGE('',*,*,#686,.F.);
#864=ORIENTED_EDGE('',*,*,#690,.T.);
#865=ORIENTED_EDGE('',*,*,#691,.T.);
#866=ORIENTED_EDGE('',*,*,#692,.F.);
#867=ORIENTED_EDGE('',*,*,#693,.F.);
#868=ORIENTED_EDGE('',*,*,#694,.T.);
#869=ORIENTED_EDGE('',*,*,#693,.T.);
#870=ORIENTED_EDGE('',*,*,#695,.F.);
#871=ORIENTED_EDGE('',*,*,#696,.F.);
#872=ORIENTED_EDGE('',*,*,#697,.T.);
#873=ORIENTED_EDGE('',*,*,#696,.T.);
#874=ORIENTED_EDGE('',*,*,#698,.F.);
#875=ORIENTED_EDGE('',*,*,#699,.F.);
#876=ORIENTED_EDGE('',*,*,#700,.F.);
#877=ORIENTED_EDGE('',*,*,#699,.T.);
#878=ORIENTED_EDGE('',*,*,#701,.F.);
#879=ORIENTED_EDGE('',*,*,#702,.F.);
#880=ORIENTED_EDGE('',*,*,#703,.T.);
#881=ORIENTED_EDGE('',*,*,#702,.T.);
#882=ORIENTED_EDGE('',*,*,#704,.T.);
#883=ORIENTED_EDGE('',*,*,#683,.F.);
#884=ORIENTED_EDGE('',*,*,#705,.T.);
#885=ORIENTED_EDGE('',*,*,#706,.T.);
#886=ORIENTED_EDGE('',*,*,#707,.T.);
#887=ORIENTED_EDGE('',*,*,#706,.F.);
#888=ORIENTED_EDGE('',*,*,#708,.T.);
#889=ORIENTED_EDGE('',*,*,#671,.T.);
#890=ORIENTED_EDGE('',*,*,#709,.F.);
#891=ORIENTED_EDGE('',*,*,#710,.F.);
#892=ORIENTED_EDGE('',*,*,#711,.F.);
#893=ORIENTED_EDGE('',*,*,#710,.T.);
#894=ORIENTED_EDGE('',*,*,#712,.F.);
#895=ORIENTED_EDGE('',*,*,#691,.F.);
#896=ORIENTED_EDGE('',*,*,#685,.F.);
#897=ORIENTED_EDGE('',*,*,#651,.T.);
#898=ORIENTED_EDGE('',*,*,#638,.F.);
#899=ORIENTED_EDGE('',*,*,#642,.F.);
#900=ORIENTED_EDGE('',*,*,#645,.F.);
#901=ORIENTED_EDGE('',*,*,#648,.T.);
#902=ORIENTED_EDGE('',*,*,#667,.T.);
#903=ORIENTED_EDGE('',*,*,#664,.F.);
#904=ORIENTED_EDGE('',*,*,#661,.T.);
#905=ORIENTED_EDGE('',*,*,#658,.T.);
#906=ORIENTED_EDGE('',*,*,#654,.T.);
#907=ORIENTED_EDGE('',*,*,#669,.F.);
#908=ORIENTED_EDGE('',*,*,#708,.F.);
#909=ORIENTED_EDGE('',*,*,#711,.T.);
#910=ORIENTED_EDGE('',*,*,#690,.F.);
#911=ORIENTED_EDGE('',*,*,#694,.F.);
#912=ORIENTED_EDGE('',*,*,#697,.F.);
#913=ORIENTED_EDGE('',*,*,#700,.T.);
#914=ORIENTED_EDGE('',*,*,#703,.F.);
#915=ORIENTED_EDGE('',*,*,#682,.F.);
#916=ORIENTED_EDGE('',*,*,#679,.T.);
#917=ORIENTED_EDGE('',*,*,#676,.T.);
#918=ORIENTED_EDGE('',*,*,#672,.T.);
#919=ORIENTED_EDGE('',*,*,#688,.F.);
#920=ORIENTED_EDGE('',*,*,#707,.F.);
#921=ORIENTED_EDGE('',*,*,#687,.T.);
#922=ORIENTED_EDGE('',*,*,#689,.F.);
#923=ORIENTED_EDGE('',*,*,#674,.F.);
#924=ORIENTED_EDGE('',*,*,#678,.F.);
#925=ORIENTED_EDGE('',*,*,#681,.F.);
#926=ORIENTED_EDGE('',*,*,#684,.F.);
#927=ORIENTED_EDGE('',*,*,#704,.F.);
#928=ORIENTED_EDGE('',*,*,#701,.T.);
#929=ORIENTED_EDGE('',*,*,#698,.T.);
#930=ORIENTED_EDGE('',*,*,#695,.T.);
#931=ORIENTED_EDGE('',*,*,#692,.T.);
#932=ORIENTED_EDGE('',*,*,#712,.T.);
#933=ORIENTED_EDGE('',*,*,#709,.T.);
#934=ORIENTED_EDGE('',*,*,#670,.F.);
#935=ORIENTED_EDGE('',*,*,#656,.F.);
#936=ORIENTED_EDGE('',*,*,#660,.F.);
#937=ORIENTED_EDGE('',*,*,#663,.F.);
#938=ORIENTED_EDGE('',*,*,#666,.F.);
#939=ORIENTED_EDGE('',*,*,#668,.T.);
#940=ORIENTED_EDGE('',*,*,#649,.T.);
#941=ORIENTED_EDGE('',*,*,#646,.T.);
#942=ORIENTED_EDGE('',*,*,#643,.T.);
#943=ORIENTED_EDGE('',*,*,#640,.T.);
#944=ORIENTED_EDGE('',*,*,#653,.T.);
#945=ORIENTED_EDGE('',*,*,#705,.F.);
#946=ORIENTED_EDGE('',*,*,#713,.T.);
#947=ORIENTED_EDGE('',*,*,#713,.F.);
#948=ORIENTED_EDGE('',*,*,#714,.T.);
#949=ORIENTED_EDGE('',*,*,#715,.T.);
#950=ORIENTED_EDGE('',*,*,#714,.F.);
#951=ORIENTED_EDGE('',*,*,#715,.F.);
#952=ORIENTED_EDGE('',*,*,#716,.T.);
#953=ORIENTED_EDGE('',*,*,#716,.F.);
#954=ORIENTED_EDGE('',*,*,#717,.T.);
#955=ORIENTED_EDGE('',*,*,#718,.T.);
#956=ORIENTED_EDGE('',*,*,#717,.F.);
#957=ORIENTED_EDGE('',*,*,#718,.F.);
#958=ORIENTED_EDGE('',*,*,#719,.F.);
#959=ORIENTED_EDGE('',*,*,#720,.T.);
#960=ORIENTED_EDGE('',*,*,#721,.F.);
#961=ORIENTED_EDGE('',*,*,#720,.F.);
#962=ORIENTED_EDGE('',*,*,#722,.F.);
#963=ORIENTED_EDGE('',*,*,#723,.T.);
#964=ORIENTED_EDGE('',*,*,#724,.T.);
#965=ORIENTED_EDGE('',*,*,#723,.F.);
#966=ORIENTED_EDGE('',*,*,#725,.F.);
#967=ORIENTED_EDGE('',*,*,#726,.F.);
#968=ORIENTED_EDGE('',*,*,#727,.F.);
#969=ORIENTED_EDGE('',*,*,#728,.F.);
#970=ORIENTED_EDGE('',*,*,#724,.F.);
#971=ORIENTED_EDGE('',*,*,#721,.T.);
#972=ORIENTED_EDGE('',*,*,#726,.T.);
#973=ORIENTED_EDGE('',*,*,#729,.T.);
#974=ORIENTED_EDGE('',*,*,#730,.F.);
#975=ORIENTED_EDGE('',*,*,#731,.F.);
#976=ORIENTED_EDGE('',*,*,#725,.T.);
#977=ORIENTED_EDGE('',*,*,#732,.T.);
#978=ORIENTED_EDGE('',*,*,#733,.F.);
#979=ORIENTED_EDGE('',*,*,#729,.F.);
#980=ORIENTED_EDGE('',*,*,#727,.T.);
#981=ORIENTED_EDGE('',*,*,#731,.T.);
#982=ORIENTED_EDGE('',*,*,#734,.F.);
#983=ORIENTED_EDGE('',*,*,#735,.F.);
#984=ORIENTED_EDGE('',*,*,#728,.T.);
#985=ORIENTED_EDGE('',*,*,#735,.T.);
#986=ORIENTED_EDGE('',*,*,#736,.F.);
#987=ORIENTED_EDGE('',*,*,#732,.F.);
#988=ORIENTED_EDGE('',*,*,#733,.T.);
#989=ORIENTED_EDGE('',*,*,#736,.T.);
#990=ORIENTED_EDGE('',*,*,#734,.T.);
#991=ORIENTED_EDGE('',*,*,#730,.T.);
#992=ORIENTED_EDGE('',*,*,#719,.T.);
#993=ORIENTED_EDGE('',*,*,#722,.T.);
#994=ORIENTED_EDGE('',*,*,#737,.T.);
#995=ORIENTED_EDGE('',*,*,#738,.T.);
#996=ORIENTED_EDGE('',*,*,#739,.F.);
#997=ORIENTED_EDGE('',*,*,#740,.F.);
#998=ORIENTED_EDGE('',*,*,#741,.T.);
#999=ORIENTED_EDGE('',*,*,#742,.T.);
#1000=ORIENTED_EDGE('',*,*,#743,.F.);
#1001=ORIENTED_EDGE('',*,*,#744,.F.);
#1002=ORIENTED_EDGE('',*,*,#743,.T.);
#1003=ORIENTED_EDGE('',*,*,#745,.T.);
#1004=ORIENTED_EDGE('',*,*,#746,.T.);
#1005=ORIENTED_EDGE('',*,*,#739,.T.);
#1006=ORIENTED_EDGE('',*,*,#747,.T.);
#1007=ORIENTED_EDGE('',*,*,#748,.F.);
#1008=ORIENTED_EDGE('',*,*,#749,.T.);
#1009=ORIENTED_EDGE('',*,*,#750,.T.);
#1010=ORIENTED_EDGE('',*,*,#751,.T.);
#1011=ORIENTED_EDGE('',*,*,#752,.T.);
#1012=ORIENTED_EDGE('',*,*,#745,.F.);
#1013=ORIENTED_EDGE('',*,*,#742,.F.);
#1014=ORIENTED_EDGE('',*,*,#740,.T.);
#1015=ORIENTED_EDGE('',*,*,#746,.F.);
#1016=ORIENTED_EDGE('',*,*,#752,.F.);
#1017=ORIENTED_EDGE('',*,*,#753,.T.);
#1018=ORIENTED_EDGE('',*,*,#750,.F.);
#1019=ORIENTED_EDGE('',*,*,#754,.T.);
#1020=ORIENTED_EDGE('',*,*,#755,.F.);
#1021=ORIENTED_EDGE('',*,*,#754,.F.);
#1022=ORIENTED_EDGE('',*,*,#756,.T.);
#1023=ORIENTED_EDGE('',*,*,#757,.F.);
#1024=ORIENTED_EDGE('',*,*,#747,.F.);
#1025=ORIENTED_EDGE('',*,*,#738,.F.);
#1026=ORIENTED_EDGE('',*,*,#749,.F.);
#1027=ORIENTED_EDGE('',*,*,#758,.T.);
#1028=ORIENTED_EDGE('',*,*,#759,.T.);
#1029=ORIENTED_EDGE('',*,*,#758,.F.);
#1030=ORIENTED_EDGE('',*,*,#737,.F.);
#1031=ORIENTED_EDGE('',*,*,#753,.F.);
#1032=ORIENTED_EDGE('',*,*,#751,.F.);
#1033=ORIENTED_EDGE('',*,*,#741,.F.);
#1034=ORIENTED_EDGE('',*,*,#760,.F.);
#1035=ORIENTED_EDGE('',*,*,#756,.F.);
#1036=ORIENTED_EDGE('',*,*,#759,.F.);
#1037=ORIENTED_EDGE('',*,*,#755,.T.);
#1038=ORIENTED_EDGE('',*,*,#760,.T.);
#1039=ORIENTED_EDGE('',*,*,#744,.T.);
#1040=ORIENTED_EDGE('',*,*,#748,.T.);
#1041=ORIENTED_EDGE('',*,*,#757,.T.);
#1042=ORIENTED_EDGE('',*,*,#761,.F.);
#1043=ORIENTED_EDGE('',*,*,#762,.F.);
#1044=ORIENTED_EDGE('',*,*,#763,.F.);
#1045=ORIENTED_EDGE('',*,*,#764,.F.);
#1046=ORIENTED_EDGE('',*,*,#765,.T.);
#1047=ORIENTED_EDGE('',*,*,#762,.T.);
#1048=ORIENTED_EDGE('',*,*,#766,.T.);
#1049=ORIENTED_EDGE('',*,*,#767,.T.);
#1050=ORIENTED_EDGE('',*,*,#768,.T.);
#1051=ORIENTED_EDGE('',*,*,#769,.F.);
#1052=ORIENTED_EDGE('',*,*,#770,.F.);
#1053=ORIENTED_EDGE('',*,*,#766,.F.);
#1054=ORIENTED_EDGE('',*,*,#761,.T.);
#1055=ORIENTED_EDGE('',*,*,#763,.T.);
#1056=ORIENTED_EDGE('',*,*,#768,.F.);
#1057=ORIENTED_EDGE('',*,*,#771,.T.);
#1058=ORIENTED_EDGE('',*,*,#772,.F.);
#1059=ORIENTED_EDGE('',*,*,#773,.F.);
#1060=ORIENTED_EDGE('',*,*,#774,.F.);
#1061=ORIENTED_EDGE('',*,*,#775,.F.);
#1062=ORIENTED_EDGE('',*,*,#776,.T.);
#1063=ORIENTED_EDGE('',*,*,#777,.T.);
#1064=ORIENTED_EDGE('',*,*,#764,.T.);
#1065=ORIENTED_EDGE('',*,*,#772,.T.);
#1066=ORIENTED_EDGE('',*,*,#778,.T.);
#1067=ORIENTED_EDGE('',*,*,#775,.T.);
#1068=ORIENTED_EDGE('',*,*,#779,.T.);
#1069=ORIENTED_EDGE('',*,*,#780,.T.);
#1070=ORIENTED_EDGE('',*,*,#781,.T.);
#1071=ORIENTED_EDGE('',*,*,#779,.F.);
#1072=ORIENTED_EDGE('',*,*,#774,.T.);
#1073=ORIENTED_EDGE('',*,*,#782,.T.);
#1074=ORIENTED_EDGE('',*,*,#783,.F.);
#1075=ORIENTED_EDGE('',*,*,#784,.T.);
#1076=ORIENTED_EDGE('',*,*,#780,.F.);
#1077=ORIENTED_EDGE('',*,*,#784,.F.);
#1078=ORIENTED_EDGE('',*,*,#785,.F.);
#1079=ORIENTED_EDGE('',*,*,#776,.F.);
#1080=ORIENTED_EDGE('',*,*,#778,.F.);
#1081=ORIENTED_EDGE('',*,*,#771,.F.);
#1082=ORIENTED_EDGE('',*,*,#767,.F.);
#1083=ORIENTED_EDGE('',*,*,#770,.T.);
#1084=ORIENTED_EDGE('',*,*,#786,.F.);
#1085=ORIENTED_EDGE('',*,*,#765,.F.);
#1086=ORIENTED_EDGE('',*,*,#777,.F.);
#1087=ORIENTED_EDGE('',*,*,#781,.F.);
#1088=ORIENTED_EDGE('',*,*,#785,.T.);
#1089=ORIENTED_EDGE('',*,*,#769,.T.);
#1090=ORIENTED_EDGE('',*,*,#786,.T.);
#1091=ORIENTED_EDGE('',*,*,#782,.F.);
#1092=ORIENTED_EDGE('',*,*,#773,.T.);
#1093=ORIENTED_EDGE('',*,*,#783,.T.);
#1094=ORIENTED_EDGE('',*,*,#787,.T.);
#1095=ORIENTED_EDGE('',*,*,#787,.F.);
#1096=ORIENTED_EDGE('',*,*,#788,.T.);
#1097=ORIENTED_EDGE('',*,*,#789,.T.);
#1098=ORIENTED_EDGE('',*,*,#788,.F.);
#1099=ORIENTED_EDGE('',*,*,#789,.F.);
#1100=ORIENTED_EDGE('',*,*,#790,.T.);
#1101=ORIENTED_EDGE('',*,*,#791,.T.);
#1102=ORIENTED_EDGE('',*,*,#790,.F.);
#1103=ORIENTED_EDGE('',*,*,#792,.T.);
#1104=ORIENTED_EDGE('',*,*,#793,.F.);
#1105=ORIENTED_EDGE('',*,*,#792,.F.);
#1106=ORIENTED_EDGE('',*,*,#794,.F.);
#1107=ORIENTED_EDGE('',*,*,#795,.T.);
#1108=ORIENTED_EDGE('',*,*,#791,.F.);
#1109=ORIENTED_EDGE('',*,*,#795,.F.);
#1110=ORIENTED_EDGE('',*,*,#793,.T.);
#1111=ORIENTED_EDGE('',*,*,#794,.T.);
#1112=PLANE('',#1325);
#1113=PLANE('',#1329);
#1114=PLANE('',#1330);
#1115=PLANE('',#1331);
#1116=PLANE('',#1332);
#1117=PLANE('',#1336);
#1118=PLANE('',#1337);
#1119=PLANE('',#1341);
#1120=PLANE('',#1342);
#1121=PLANE('',#1346);
#1122=PLANE('',#1347);
#1123=PLANE('',#1351);
#1124=PLANE('',#1352);
#1125=PLANE('',#1356);
#1126=PLANE('',#1357);
#1127=PLANE('',#1367);
#1128=PLANE('',#1368);
#1129=PLANE('',#1369);
#1130=PLANE('',#1371);
#1131=PLANE('',#1375);
#1132=PLANE('',#1377);
#1133=PLANE('',#1381);
#1134=PLANE('',#1389);
#1135=PLANE('',#1390);
#1136=PLANE('',#1391);
#1137=PLANE('',#1392);
#1138=PLANE('',#1393);
#1139=PLANE('',#1394);
#1140=PLANE('',#1396);
#1141=PLANE('',#1397);
#1142=PLANE('',#1398);
#1143=PLANE('',#1403);
#1144=PLANE('',#1408);
#1145=PLANE('',#1411);
#1146=PLANE('',#1415);
#1147=PLANE('',#1416);
#1148=PLANE('',#1423);
#1149=PLANE('',#1424);
#1150=PLANE('',#1431);
#1151=PLANE('',#1432);
#1152=PLANE('',#1433);
#1153=PLANE('',#1435);
#1154=PLANE('',#1439);
#1155=PLANE('',#1441);
#1156=PLANE('',#1448);
#1157=ADVANCED_FACE('',(#161),#1112,.T.);
#1158=ADVANCED_FACE('',(#162),#137,.F.);
#1159=ADVANCED_FACE('',(#163),#1113,.T.);
#1160=ADVANCED_FACE('',(#164),#1114,.T.);
#1161=ADVANCED_FACE('',(#165),#1115,.T.);
#1162=ADVANCED_FACE('',(#166),#1116,.F.);
#1163=ADVANCED_FACE('',(#167),#138,.F.);
#1164=ADVANCED_FACE('',(#168),#1117,.F.);
#1165=ADVANCED_FACE('',(#169),#1118,.F.);
#1166=ADVANCED_FACE('',(#170),#139,.F.);
#1167=ADVANCED_FACE('',(#171),#1119,.F.);
#1168=ADVANCED_FACE('',(#172),#1120,.F.);
#1169=ADVANCED_FACE('',(#173),#140,.F.);
#1170=ADVANCED_FACE('',(#174),#1121,.F.);
#1171=ADVANCED_FACE('',(#175),#1122,.F.);
#1172=ADVANCED_FACE('',(#176),#141,.F.);
#1173=ADVANCED_FACE('',(#177),#1123,.F.);
#1174=ADVANCED_FACE('',(#178),#1124,.T.);
#1175=ADVANCED_FACE('',(#179),#142,.F.);
#1176=ADVANCED_FACE('',(#180),#1125,.T.);
#1177=ADVANCED_FACE('',(#181),#1126,.T.);
#1178=ADVANCED_FACE('',(#182),#143,.F.);
#1179=ADVANCED_FACE('',(#183),#144,.F.);
#1180=ADVANCED_FACE('',(#184),#145,.F.);
#1181=ADVANCED_FACE('',(#185),#1127,.T.);
#1182=ADVANCED_FACE('',(#186,#75),#1128,.T.);
#1183=ADVANCED_FACE('',(#187,#76),#1129,.F.);
#1184=ADVANCED_FACE('',(#188),#1130,.F.);
#1185=ADVANCED_FACE('',(#189),#146,.T.);
#1186=ADVANCED_FACE('',(#190),#1131,.T.);
#1187=ADVANCED_FACE('',(#191),#1132,.T.);
#1188=ADVANCED_FACE('',(#192),#147,.T.);
#1189=ADVANCED_FACE('',(#193),#1133,.T.);
#1190=ADVANCED_FACE('',(#194),#148,.F.);
#1191=ADVANCED_FACE('',(#195),#149,.F.);
#1192=ADVANCED_FACE('',(#196,#77,#78),#1134,.F.);
#1193=ADVANCED_FACE('',(#197),#1135,.T.);
#1194=ADVANCED_FACE('',(#198),#1136,.T.);
#1195=ADVANCED_FACE('',(#199),#1137,.T.);
#1196=ADVANCED_FACE('',(#200),#1138,.T.);
#1197=ADVANCED_FACE('',(#201,#79,#80),#1139,.T.);
#1198=ADVANCED_FACE('',(#202),#1140,.T.);
#1199=ADVANCED_FACE('',(#203),#1141,.F.);
#1200=ADVANCED_FACE('',(#204,#81,#82),#1142,.T.);
#1201=ADVANCED_FACE('',(#205),#1143,.T.);
#1202=ADVANCED_FACE('',(#206),#150,.T.);
#1203=ADVANCED_FACE('',(#207),#151,.F.);
#1204=ADVANCED_FACE('',(#208),#1144,.T.);
#1205=ADVANCED_FACE('',(#209),#152,.F.);
#1206=ADVANCED_FACE('',(#210,#83,#84),#1145,.F.);
#1207=ADVANCED_FACE('',(#211),#153,.T.);
#1208=ADVANCED_FACE('',(#212),#1146,.F.);
#1209=ADVANCED_FACE('',(#213),#1147,.T.);
#1210=ADVANCED_FACE('',(#214),#154,.F.);
#1211=ADVANCED_FACE('',(#215),#155,.T.);
#1212=ADVANCED_FACE('',(#216),#1148,.T.);
#1213=ADVANCED_FACE('',(#217,#85),#1149,.F.);
#1214=ADVANCED_FACE('',(#218),#156,.F.);
#1215=ADVANCED_FACE('',(#219),#157,.F.);
#1216=ADVANCED_FACE('',(#220),#1150,.T.);
#1217=ADVANCED_FACE('',(#221),#1151,.F.);
#1218=ADVANCED_FACE('',(#222,#86),#1152,.T.);
#1219=ADVANCED_FACE('',(#223),#1153,.T.);
#1220=ADVANCED_FACE('',(#224),#158,.T.);
#1221=ADVANCED_FACE('',(#225),#1154,.T.);
#1222=ADVANCED_FACE('',(#226,#87),#1155,.T.);
#1223=ADVANCED_FACE('',(#227),#159,.T.);
#1224=ADVANCED_FACE('',(#228),#160,.F.);
#1225=ADVANCED_FACE('',(#229,#88),#1156,.T.);
#1226=CLOSED_SHELL('',(#1157,#1158,#1159,#1160,#1161,#1162,#1163,#1164,
#1165,#1166,#1167,#1168,#1169,#1170,#1171,#1172,#1173,#1174,#1175,#1176,
#1177,#1178,#1179,#1180,#1181,#1182,#1183));
#1227=CLOSED_SHELL('',(#1184,#1185,#1186));
#1228=CLOSED_SHELL('',(#1187,#1188,#1189));
#1229=CLOSED_SHELL('',(#1190,#1191,#1192,#1193,#1194,#1195,#1196,#1197));
#1230=CLOSED_SHELL('',(#1198,#1199,#1200,#1201,#1202,#1203,#1204,#1205,
#1206,#1207));
#1231=CLOSED_SHELL('',(#1208,#1209,#1210,#1211,#1212,#1213,#1214,#1215,
#1216,#1217,#1218));
#1232=CLOSED_SHELL('',(#1219,#1220,#1221));
#1233=CLOSED_SHELL('',(#1222,#1223,#1224,#1225));
#1234=DERIVED_UNIT_ELEMENT(#1250,1.);
#1235=DERIVED_UNIT_ELEMENT(#2205,-3.);
#1236=DERIVED_UNIT_ELEMENT(#1250,1.);
#1237=DERIVED_UNIT_ELEMENT(#2205,-3.);
#1238=DERIVED_UNIT_ELEMENT(#1250,1.);
#1239=DERIVED_UNIT_ELEMENT(#2205,-3.);
#1240=DERIVED_UNIT_ELEMENT(#1250,1.);
#1241=DERIVED_UNIT_ELEMENT(#2205,-3.);
#1242=DERIVED_UNIT_ELEMENT(#1250,1.);
#1243=DERIVED_UNIT_ELEMENT(#2205,-3.);
#1244=DERIVED_UNIT_ELEMENT(#1250,1.);
#1245=DERIVED_UNIT_ELEMENT(#2205,-3.);
#1246=DERIVED_UNIT_ELEMENT(#1250,1.);
#1247=DERIVED_UNIT_ELEMENT(#2205,-3.);
#1248=DERIVED_UNIT_ELEMENT(#1250,1.);
#1249=DERIVED_UNIT_ELEMENT(#2205,-3.);
#1250=(
MASS_UNIT()
NAMED_UNIT(*)
SI_UNIT(.KILO.,.GRAM.)
);
#1251=DERIVED_UNIT((#1234,#1235));
#1252=DERIVED_UNIT((#1236,#1237));
#1253=DERIVED_UNIT((#1238,#1239));
#1254=DERIVED_UNIT((#1240,#1241));
#1255=DERIVED_UNIT((#1242,#1243));
#1256=DERIVED_UNIT((#1244,#1245));
#1257=DERIVED_UNIT((#1246,#1247));
#1258=DERIVED_UNIT((#1248,#1249));
#1259=MEASURE_REPRESENTATION_ITEM('density measure',
POSITIVE_RATIO_MEASURE(7850.),#1251);
#1260=MEASURE_REPRESENTATION_ITEM('density measure',
POSITIVE_RATIO_MEASURE(7850.),#1252);
#1261=MEASURE_REPRESENTATION_ITEM('density measure',
POSITIVE_RATIO_MEASURE(7850.),#1253);
#1262=MEASURE_REPRESENTATION_ITEM('density measure',
POSITIVE_RATIO_MEASURE(7850.),#1254);
#1263=MEASURE_REPRESENTATION_ITEM('density measure',
POSITIVE_RATIO_MEASURE(7850.),#1255);
#1264=MEASURE_REPRESENTATION_ITEM('density measure',
POSITIVE_RATIO_MEASURE(7850.),#1256);
#1265=MEASURE_REPRESENTATION_ITEM('density measure',
POSITIVE_RATIO_MEASURE(7850.),#1257);
#1266=MEASURE_REPRESENTATION_ITEM('density measure',
POSITIVE_RATIO_MEASURE(7850.),#1258);
#1267=PROPERTY_DEFINITION_REPRESENTATION(#1307,#1283);
#1268=PROPERTY_DEFINITION_REPRESENTATION(#1308,#1284);
#1269=PROPERTY_DEFINITION_REPRESENTATION(#1309,#1285);
#1270=PROPERTY_DEFINITION_REPRESENTATION(#1310,#1286);
#1271=PROPERTY_DEFINITION_REPRESENTATION(#1311,#1287);
#1272=PROPERTY_DEFINITION_REPRESENTATION(#1312,#1288);
#1273=PROPERTY_DEFINITION_REPRESENTATION(#1313,#1289);
#1274=PROPERTY_DEFINITION_REPRESENTATION(#1314,#1290);
#1275=PROPERTY_DEFINITION_REPRESENTATION(#1315,#1291);
#1276=PROPERTY_DEFINITION_REPRESENTATION(#1316,#1292);
#1277=PROPERTY_DEFINITION_REPRESENTATION(#1317,#1293);
#1278=PROPERTY_DEFINITION_REPRESENTATION(#1318,#1294);
#1279=PROPERTY_DEFINITION_REPRESENTATION(#1319,#1295);
#1280=PROPERTY_DEFINITION_REPRESENTATION(#1320,#1296);
#1281=PROPERTY_DEFINITION_REPRESENTATION(#1321,#1297);
#1282=PROPERTY_DEFINITION_REPRESENTATION(#1322,#1298);
#1283=REPRESENTATION('material name',(#1299),#2195);
#1284=REPRESENTATION('density',(#1259),#2195);
#1285=REPRESENTATION('material name',(#1300),#2196);
#1286=REPRESENTATION('density',(#1260),#2196);
#1287=REPRESENTATION('material name',(#1301),#2197);
#1288=REPRESENTATION('density',(#1261),#2197);
#1289=REPRESENTATION('material name',(#1302),#2198);
#1290=REPRESENTATION('density',(#1262),#2198);
#1291=REPRESENTATION('material name',(#1303),#2199);
#1292=REPRESENTATION('density',(#1263),#2199);
#1293=REPRESENTATION('material name',(#1304),#2200);
#1294=REPRESENTATION('density',(#1264),#2200);
#1295=REPRESENTATION('material name',(#1305),#2201);
#1296=REPRESENTATION('density',(#1265),#2201);
#1297=REPRESENTATION('material name',(#1306),#2202);
#1298=REPRESENTATION('density',(#1266),#2202);
#1299=DESCRIPTIVE_REPRESENTATION_ITEM('Steel','Steel');
#1300=DESCRIPTIVE_REPRESENTATION_ITEM('Steel','Steel');
#1301=DESCRIPTIVE_REPRESENTATION_ITEM('Steel','Steel');
#1302=DESCRIPTIVE_REPRESENTATION_ITEM('Steel','Steel');
#1303=DESCRIPTIVE_REPRESENTATION_ITEM('Steel','Steel');
#1304=DESCRIPTIVE_REPRESENTATION_ITEM('Steel','Steel');
#1305=DESCRIPTIVE_REPRESENTATION_ITEM('Steel','Steel');
#1306=DESCRIPTIVE_REPRESENTATION_ITEM('Steel','Steel');
#1307=PROPERTY_DEFINITION('material property','material name',#2245);
#1308=PROPERTY_DEFINITION('material property','density of part',#2245);
#1309=PROPERTY_DEFINITION('material property','material name',#2246);
#1310=PROPERTY_DEFINITION('material property','density of part',#2246);
#1311=PROPERTY_DEFINITION('material property','material name',#2247);
#1312=PROPERTY_DEFINITION('material property','density of part',#2247);
#1313=PROPERTY_DEFINITION('material property','material name',#2248);
#1314=PROPERTY_DEFINITION('material property','density of part',#2248);
#1315=PROPERTY_DEFINITION('material property','material name',#2249);
#1316=PROPERTY_DEFINITION('material property','density of part',#2249);
#1317=PROPERTY_DEFINITION('material property','material name',#2250);
#1318=PROPERTY_DEFINITION('material property','density of part',#2250);
#1319=PROPERTY_DEFINITION('material property','material name',#2251);
#1320=PROPERTY_DEFINITION('material property','density of part',#2251);
#1321=PROPERTY_DEFINITION('material property','material name',#2252);
#1322=PROPERTY_DEFINITION('material property','density of part',#2252);
#1323=AXIS2_PLACEMENT_3D('',#1835,#1457,#1458);
#1324=AXIS2_PLACEMENT_3D('',#1836,#1459,#1460);
#1325=AXIS2_PLACEMENT_3D('',#1837,#1461,#1462);
#1326=AXIS2_PLACEMENT_3D('',#1846,#1467,#1468);
#1327=AXIS2_PLACEMENT_3D('',#1848,#1469,#1470);
#1328=AXIS2_PLACEMENT_3D('',#1850,#1471,#1472);
#1329=AXIS2_PLACEMENT_3D('',#1852,#1474,#1475);
#1330=AXIS2_PLACEMENT_3D('',#1858,#1479,#1480);
#1331=AXIS2_PLACEMENT_3D('',#1864,#1484,#1485);
#1332=AXIS2_PLACEMENT_3D('',#1870,#1489,#1490);
#1333=AXIS2_PLACEMENT_3D('',#1879,#1495,#1496);
#1334=AXIS2_PLACEMENT_3D('',#1881,#1497,#1498);
#1335=AXIS2_PLACEMENT_3D('',#1884,#1500,#1501);
#1336=AXIS2_PLACEMENT_3D('',#1885,#1502,#1503);
#1337=AXIS2_PLACEMENT_3D('',#1891,#1507,#1508);
#1338=AXIS2_PLACEMENT_3D('',#1897,#1512,#1513);
#1339=AXIS2_PLACEMENT_3D('',#1898,#1514,#1515);
#1340=AXIS2_PLACEMENT_3D('',#1899,#1516,#1517);
#1341=AXIS2_PLACEMENT_3D('',#1900,#1518,#1519);
#1342=AXIS2_PLACEMENT_3D('',#1906,#1523,#1524);
#1343=AXIS2_PLACEMENT_3D('',#1915,#1529,#1530);
#1344=AXIS2_PLACEMENT_3D('',#1917,#1531,#1532);
#1345=AXIS2_PLACEMENT_3D('',#1920,#1534,#1535);
#1346=AXIS2_PLACEMENT_3D('',#1921,#1536,#1537);
#1347=AXIS2_PLACEMENT_3D('',#1927,#1541,#1542);
#1348=AXIS2_PLACEMENT_3D('',#1933,#1546,#1547);
#1349=AXIS2_PLACEMENT_3D('',#1935,#1548,#1549);
#1350=AXIS2_PLACEMENT_3D('',#1938,#1551,#1552);
#1351=AXIS2_PLACEMENT_3D('',#1939,#1553,#1554);
#1352=AXIS2_PLACEMENT_3D('',#1942,#1557,#1558);
#1353=AXIS2_PLACEMENT_3D('',#1951,#1563,#1564);
#1354=AXIS2_PLACEMENT_3D('',#1953,#1565,#1566);
#1355=AXIS2_PLACEMENT_3D('',#1955,#1567,#1568);
#1356=AXIS2_PLACEMENT_3D('',#1957,#1570,#1571);
#1357=AXIS2_PLACEMENT_3D('',#1963,#1575,#1576);
#1358=AXIS2_PLACEMENT_3D('',#1969,#1580,#1581);
#1359=AXIS2_PLACEMENT_3D('',#1970,#1582,#1583);
#1360=AXIS2_PLACEMENT_3D('',#1971,#1584,#1585);
#1361=AXIS2_PLACEMENT_3D('',#1972,#1586,#1587);
#1362=AXIS2_PLACEMENT_3D('',#1974,#1588,#1589);
#1363=AXIS2_PLACEMENT_3D('',#1977,#1591,#1592);
#1364=AXIS2_PLACEMENT_3D('',#1978,#1593,#1594);
#1365=AXIS2_PLACEMENT_3D('',#1980,#1595,#1596);
#1366=AXIS2_PLACEMENT_3D('',#1982,#1597,#1598);
#1367=AXIS2_PLACEMENT_3D('',#1984,#1600,#1601);
#1368=AXIS2_PLACEMENT_3D('',#1987,#1604,#1605);
#1369=AXIS2_PLACEMENT_3D('',#1988,#1606,#1607);
#1370=AXIS2_PLACEMENT_3D('',#1989,#1608,#1609);
#1371=AXIS2_PLACEMENT_3D('',#1990,#1610,#1611);
#1372=AXIS2_PLACEMENT_3D('',#1992,#1612,#1613);
#1373=AXIS2_PLACEMENT_3D('',#1993,#1614,#1615);
#1374=AXIS2_PLACEMENT_3D('',#1996,#1617,#1618);
#1375=AXIS2_PLACEMENT_3D('',#1997,#1619,#1620);
#1376=AXIS2_PLACEMENT_3D('',#1998,#1621,#1622);
#1377=AXIS2_PLACEMENT_3D('',#1999,#1623,#1624);
#1378=AXIS2_PLACEMENT_3D('',#2001,#1625,#1626);
#1379=AXIS2_PLACEMENT_3D('',#2002,#1627,#1628);
#1380=AXIS2_PLACEMENT_3D('',#2005,#1630,#1631);
#1381=AXIS2_PLACEMENT_3D('',#2006,#1632,#1633);
#1382=AXIS2_PLACEMENT_3D('',#2007,#1634,#1635);
#1383=AXIS2_PLACEMENT_3D('',#2008,#1636,#1637);
#1384=AXIS2_PLACEMENT_3D('',#2010,#1638,#1639);
#1385=AXIS2_PLACEMENT_3D('',#2013,#1641,#1642);
#1386=AXIS2_PLACEMENT_3D('',#2014,#1643,#1644);
#1387=AXIS2_PLACEMENT_3D('',#2016,#1645,#1646);
#1388=AXIS2_PLACEMENT_3D('',#2019,#1648,#1649);
#1389=AXIS2_PLACEMENT_3D('',#2020,#1650,#1651);
#1390=AXIS2_PLACEMENT_3D('',#2029,#1656,#1657);
#1391=AXIS2_PLACEMENT_3D('',#2035,#1661,#1662);
#1392=AXIS2_PLACEMENT_3D('',#2039,#1665,#1666);
#1393=AXIS2_PLACEMENT_3D('',#2043,#1669,#1670);
#1394=AXIS2_PLACEMENT_3D('',#2045,#1672,#1673);
#1395=AXIS2_PLACEMENT_3D('',#2046,#1674,#1675);
#1396=AXIS2_PLACEMENT_3D('',#2047,#1676,#1677);
#1397=AXIS2_PLACEMENT_3D('',#2056,#1682,#1683);
#1398=AXIS2_PLACEMENT_3D('',#2065,#1688,#1689);
#1399=AXIS2_PLACEMENT_3D('',#2068,#1691,#1692);
#1400=AXIS2_PLACEMENT_3D('',#2071,#1694,#1695);
#1401=AXIS2_PLACEMENT_3D('',#2073,#1696,#1697);
#1402=AXIS2_PLACEMENT_3D('',#2075,#1698,#1699);
#1403=AXIS2_PLACEMENT_3D('',#2076,#1700,#1701);
#1404=AXIS2_PLACEMENT_3D('',#2080,#1704,#1705);
#1405=AXIS2_PLACEMENT_3D('',#2081,#1706,#1707);
#1406=AXIS2_PLACEMENT_3D('',#2082,#1708,#1709);
#1407=AXIS2_PLACEMENT_3D('',#2085,#1711,#1712);
#1408=AXIS2_PLACEMENT_3D('',#2086,#1713,#1714);
#1409=AXIS2_PLACEMENT_3D('',#2090,#1717,#1718);
#1410=AXIS2_PLACEMENT_3D('',#2093,#1720,#1721);
#1411=AXIS2_PLACEMENT_3D('',#2094,#1722,#1723);
#1412=AXIS2_PLACEMENT_3D('',#2095,#1724,#1725);
#1413=AXIS2_PLACEMENT_3D('',#2096,#1726,#1727);
#1414=AXIS2_PLACEMENT_3D('',#2097,#1728,#1729);
#1415=AXIS2_PLACEMENT_3D('',#2098,#1730,#1731);
#1416=AXIS2_PLACEMENT_3D('',#2109,#1737,#1738);
#1417=AXIS2_PLACEMENT_3D('',#2111,#1739,#1740);
#1418=AXIS2_PLACEMENT_3D('',#2114,#1742,#1743);
#1419=AXIS2_PLACEMENT_3D('',#2115,#1744,#1745);
#1420=AXIS2_PLACEMENT_3D('',#2117,#1746,#1747);
#1421=AXIS2_PLACEMENT_3D('',#2119,#1749,#1750);
#1422=AXIS2_PLACEMENT_3D('',#2122,#1752,#1753);
#1423=AXIS2_PLACEMENT_3D('',#2123,#1754,#1755);
#1424=AXIS2_PLACEMENT_3D('',#2132,#1760,#1761);
#1425=AXIS2_PLACEMENT_3D('',#2136,#1764,#1765);
#1426=AXIS2_PLACEMENT_3D('',#2138,#1766,#1767);
#1427=AXIS2_PLACEMENT_3D('',#2139,#1768,#1769);
#1428=AXIS2_PLACEMENT_3D('',#2142,#1771,#1772);
#1429=AXIS2_PLACEMENT_3D('',#2143,#1773,#1774);
#1430=AXIS2_PLACEMENT_3D('',#2145,#1775,#1776);
#1431=AXIS2_PLACEMENT_3D('',#2147,#1778,#1779);
#1432=AXIS2_PLACEMENT_3D('',#2149,#1781,#1782);
#1433=AXIS2_PLACEMENT_3D('',#2151,#1784,#1785);
#1434=AXIS2_PLACEMENT_3D('',#2152,#1786,#1787);
#1435=AXIS2_PLACEMENT_3D('',#2153,#1788,#1789);
#1436=AXIS2_PLACEMENT_3D('',#2155,#1790,#1791);
#1437=AXIS2_PLACEMENT_3D('',#2156,#1792,#1793);
#1438=AXIS2_PLACEMENT_3D('',#2159,#1795,#1796);
#1439=AXIS2_PLACEMENT_3D('',#2160,#1797,#1798);
#1440=AXIS2_PLACEMENT_3D('',#2161,#1799,#1800);
#1441=AXIS2_PLACEMENT_3D('',#2162,#1801,#1802);
#1442=AXIS2_PLACEMENT_3D('',#2164,#1803,#1804);
#1443=AXIS2_PLACEMENT_3D('',#2166,#1805,#1806);
#1444=AXIS2_PLACEMENT_3D('',#2167,#1807,#1808);
#1445=AXIS2_PLACEMENT_3D('',#2170,#1810,#1811);
#1446=AXIS2_PLACEMENT_3D('',#2171,#1812,#1813);
#1447=AXIS2_PLACEMENT_3D('',#2173,#1814,#1815);
#1448=AXIS2_PLACEMENT_3D('',#2175,#1817,#1818);
#1449=AXIS2_PLACEMENT_3D('',#2176,#1819,#1820);
#1450=AXIS2_PLACEMENT_3D('',#2177,#1821,#1822);
#1451=AXIS2_PLACEMENT_3D('',#2178,#1823,#1824);
#1452=AXIS2_PLACEMENT_3D('',#2179,#1825,#1826);
#1453=AXIS2_PLACEMENT_3D('',#2180,#1827,#1828);
#1454=AXIS2_PLACEMENT_3D('',#2181,#1829,#1830);
#1455=AXIS2_PLACEMENT_3D('',#2182,#1831,#1832);
#1456=AXIS2_PLACEMENT_3D('',#2183,#1833,#1834);
#1457=DIRECTION('axis',(0.,0.,1.));
#1458=DIRECTION('refdir',(1.,0.,0.));
#1459=DIRECTION('axis',(0.,0.,1.));
#1460=DIRECTION('refdir',(1.,0.,0.));
#1461=DIRECTION('center_axis',(0.707106781186548,0.,-0.707106781186547));
#1462=DIRECTION('ref_axis',(0.707106781186547,0.,0.707106781186548));
#1463=DIRECTION('',(0.707106781186547,0.,0.707106781186548));
#1464=DIRECTION('',(0.,-1.,0.));
#1465=DIRECTION('',(0.707106781186547,0.,0.707106781186548));
#1466=DIRECTION('',(0.,-1.,0.));
#1467=DIRECTION('center_axis',(0.,-1.,0.));
#1468=DIRECTION('ref_axis',(0.707106781186549,0.,-0.707106781186546));
#1469=DIRECTION('center_axis',(0.,1.,0.));
#1470=DIRECTION('ref_axis',(0.707106781186549,0.,-0.707106781186546));
#1471=DIRECTION('center_axis',(0.,1.,0.));
#1472=DIRECTION('ref_axis',(0.707106781186549,0.,-0.707106781186546));
#1473=DIRECTION('',(0.,-1.,0.));
#1474=DIRECTION('center_axis',(-0.707106781186548,0.,0.707106781186547));
#1475=DIRECTION('ref_axis',(-0.707106781186547,0.,-0.707106781186548));
#1476=DIRECTION('',(-0.707106781186547,0.,-0.707106781186548));
#1477=DIRECTION('',(-0.707106781186547,0.,-0.707106781186548));
#1478=DIRECTION('',(0.,-1.,0.));
#1479=DIRECTION('center_axis',(0.707106781186547,0.,0.707106781186548));
#1480=DIRECTION('ref_axis',(-0.707106781186548,0.,0.707106781186547));
#1481=DIRECTION('',(0.707106781186548,0.,-0.707106781186547));
#1482=DIRECTION('',(-0.707106781186548,0.,0.707106781186547));
#1483=DIRECTION('',(0.,-1.,0.));
#1484=DIRECTION('center_axis',(0.707106781186547,0.,0.707106781186548));
#1485=DIRECTION('ref_axis',(-0.707106781186548,0.,0.707106781186547));
#1486=DIRECTION('',(0.707106781186548,0.,-0.707106781186547));
#1487=DIRECTION('',(0.,-1.,0.));
#1488=DIRECTION('',(-0.707106781186548,0.,0.707106781186547));
#1489=DIRECTION('center_axis',(-0.707106781186548,0.,-0.707106781186547));
#1490=DIRECTION('ref_axis',(0.707106781186547,0.,-0.707106781186548));
#1491=DIRECTION('',(0.707106781186547,0.,-0.707106781186548));
#1492=DIRECTION('',(0.,-1.,0.));
#1493=DIRECTION('',(0.707106781186547,0.,-0.707106781186548));
#1494=DIRECTION('',(0.,-1.,0.));
#1495=DIRECTION('center_axis',(0.,1.,0.));
#1496=DIRECTION('ref_axis',(0.707106781186549,0.,0.707106781186546));
#1497=DIRECTION('center_axis',(0.,-1.,0.));
#1498=DIRECTION('ref_axis',(0.707106781186549,0.,0.707106781186546));
#1499=DIRECTION('',(0.,-1.,0.));
#1500=DIRECTION('center_axis',(0.,-1.,0.));
#1501=DIRECTION('ref_axis',(0.707106781186549,0.,0.707106781186546));
#1502=DIRECTION('center_axis',(0.707106781186548,0.,0.707106781186547));
#1503=DIRECTION('ref_axis',(-0.707106781186547,0.,0.707106781186548));
#1504=DIRECTION('',(-0.707106781186547,0.,0.707106781186548));
#1505=DIRECTION('',(0.,-1.,0.));
#1506=DIRECTION('',(-0.707106781186547,0.,0.707106781186548));
#1507=DIRECTION('center_axis',(-0.707106781186547,0.,0.707106781186548));
#1508=DIRECTION('ref_axis',(-0.707106781186548,0.,-0.707106781186547));
#1509=DIRECTION('',(0.707106781186548,0.,0.707106781186547));
#1510=DIRECTION('',(0.,-1.,0.));
#1511=DIRECTION('',(-0.707106781186548,0.,-0.707106781186547));
#1512=DIRECTION('center_axis',(0.,1.,0.));
#1513=DIRECTION('ref_axis',(-1.,0.,0.));
#1514=DIRECTION('center_axis',(0.,-1.,0.));
#1515=DIRECTION('ref_axis',(-1.,0.,0.));
#1516=DIRECTION('center_axis',(0.,1.,0.));
#1517=DIRECTION('ref_axis',(-1.,0.,0.));
#1518=DIRECTION('center_axis',(-0.707106781186547,0.,0.707106781186548));
#1519=DIRECTION('ref_axis',(-0.707106781186548,0.,-0.707106781186547));
#1520=DIRECTION('',(0.707106781186548,0.,0.707106781186547));
#1521=DIRECTION('',(-0.707106781186548,0.,-0.707106781186547));
#1522=DIRECTION('',(0.,-1.,0.));
#1523=DIRECTION('center_axis',(0.707106781186548,0.,0.707106781186547));
#1524=DIRECTION('ref_axis',(-0.707106781186547,0.,0.707106781186548));
#1525=DIRECTION('',(-0.707106781186547,0.,0.707106781186548));
#1526=DIRECTION('',(0.,-1.,0.));
#1527=DIRECTION('',(-0.707106781186547,0.,0.707106781186548));
#1528=DIRECTION('',(0.,-1.,0.));
#1529=DIRECTION('center_axis',(0.,1.,0.));
#1530=DIRECTION('ref_axis',(-0.707106781186549,0.,-0.707106781186546));
#1531=DIRECTION('center_axis',(0.,-1.,0.));
#1532=DIRECTION('ref_axis',(-0.707106781186549,0.,-0.707106781186546));
#1533=DIRECTION('',(0.,-1.,0.));
#1534=DIRECTION('center_axis',(0.,-1.,0.));
#1535=DIRECTION('ref_axis',(-0.707106781186549,0.,-0.707106781186546));
#1536=DIRECTION('center_axis',(-0.707106781186548,0.,-0.707106781186547));
#1537=DIRECTION('ref_axis',(0.707106781186547,0.,-0.707106781186548));
#1538=DIRECTION('',(0.707106781186547,0.,-0.707106781186548));
#1539=DIRECTION('',(0.,-1.,0.));
#1540=DIRECTION('',(0.707106781186547,0.,-0.707106781186548));
#1541=DIRECTION('center_axis',(0.707106781186547,0.,-0.707106781186548));
#1542=DIRECTION('ref_axis',(0.707106781186548,0.,0.707106781186547));
#1543=DIRECTION('',(-0.707106781186548,0.,-0.707106781186547));
#1544=DIRECTION('',(0.,-1.,0.));
#1545=DIRECTION('',(0.707106781186548,0.,0.707106781186547));
#1546=DIRECTION('center_axis',(0.,1.,0.));
#1547=DIRECTION('ref_axis',(1.,0.,0.));
#1548=DIRECTION('center_axis',(0.,1.,0.));
#1549=DIRECTION('ref_axis',(-1.,0.,0.));
#1550=DIRECTION('',(0.,-1.,0.));
#1551=DIRECTION('center_axis',(0.,1.,0.));
#1552=DIRECTION('ref_axis',(-1.,0.,0.));
#1553=DIRECTION('center_axis',(0.707106781186547,0.,-0.707106781186548));
#1554=DIRECTION('ref_axis',(0.707106781186548,0.,0.707106781186547));
#1555=DIRECTION('',(-0.707106781186548,0.,-0.707106781186547));
#1556=DIRECTION('',(0.707106781186548,0.,0.707106781186547));
#1557=DIRECTION('center_axis',(-0.707106781186548,0.,0.707106781186547));
#1558=DIRECTION('ref_axis',(-0.707106781186547,0.,-0.707106781186548));
#1559=DIRECTION('',(-0.707106781186547,0.,-0.707106781186548));
#1560=DIRECTION('',(0.,-1.,0.));
#1561=DIRECTION('',(-0.707106781186547,0.,-0.707106781186548));
#1562=DIRECTION('',(0.,-1.,0.));
#1563=DIRECTION('center_axis',(0.,-1.,0.));
#1564=DIRECTION('ref_axis',(-0.707106781186549,0.,0.707106781186546));
#1565=DIRECTION('center_axis',(0.,1.,0.));
#1566=DIRECTION('ref_axis',(-0.707106781186549,0.,0.707106781186546));
#1567=DIRECTION('center_axis',(0.,1.,0.));
#1568=DIRECTION('ref_axis',(-0.707106781186549,0.,0.707106781186546));
#1569=DIRECTION('',(0.,-1.,0.));
#1570=DIRECTION('center_axis',(0.707106781186548,0.,-0.707106781186547));
#1571=DIRECTION('ref_axis',(0.707106781186547,0.,0.707106781186548));
#1572=DIRECTION('',(0.707106781186547,0.,0.707106781186548));
#1573=DIRECTION('',(0.707106781186547,0.,0.707106781186548));
#1574=DIRECTION('',(0.,-1.,0.));
#1575=DIRECTION('center_axis',(-0.707106781186547,0.,-0.707106781186548));
#1576=DIRECTION('ref_axis',(0.707106781186548,0.,-0.707106781186547));
#1577=DIRECTION('',(-0.707106781186548,0.,0.707106781186547));
#1578=DIRECTION('',(0.707106781186548,0.,-0.707106781186547));
#1579=DIRECTION('',(0.,-1.,0.));
#1580=DIRECTION('center_axis',(0.,-1.,0.));
#1581=DIRECTION('ref_axis',(1.,0.,0.));
#1582=DIRECTION('center_axis',(0.,1.,0.));
#1583=DIRECTION('ref_axis',(1.,0.,0.));
#1584=DIRECTION('center_axis',(0.,-1.,0.));
#1585=DIRECTION('ref_axis',(1.,0.,0.));
#1586=DIRECTION('center_axis',(0.,-1.,0.));
#1587=DIRECTION('ref_axis',(1.,0.,0.));
#1588=DIRECTION('center_axis',(0.,-1.,0.));
#1589=DIRECTION('ref_axis',(-1.,0.,0.));
#1590=DIRECTION('',(0.,1.,0.));
#1591=DIRECTION('center_axis',(0.,1.,0.));
#1592=DIRECTION('ref_axis',(1.,0.,0.));
#1593=DIRECTION('center_axis',(0.,-1.,0.));
#1594=DIRECTION('ref_axis',(1.,0.,0.));
#1595=DIRECTION('center_axis',(0.,1.,0.));
#1596=DIRECTION('ref_axis',(1.,0.,0.));
#1597=DIRECTION('center_axis',(0.,1.,0.));
#1598=DIRECTION('ref_axis',(1.,0.,0.));
#1599=DIRECTION('',(0.,-1.,0.));
#1600=DIRECTION('center_axis',(-0.707106781186547,0.,-0.707106781186548));
#1601=DIRECTION('ref_axis',(0.707106781186548,0.,-0.707106781186547));
#1602=DIRECTION('',(-0.707106781186548,0.,0.707106781186547));
#1603=DIRECTION('',(0.707106781186548,0.,-0.707106781186547));
#1604=DIRECTION('center_axis',(0.,1.,0.));
#1605=DIRECTION('ref_axis',(1.,0.,0.));
#1606=DIRECTION('center_axis',(0.,1.,0.));
#1607=DIRECTION('ref_axis',(1.,0.,0.));
#1608=DIRECTION('axis',(0.,0.,1.));
#1609=DIRECTION('refdir',(1.,0.,0.));
#1610=DIRECTION('center_axis',(0.,1.,0.));
#1611=DIRECTION('ref_axis',(1.,0.,0.));
#1612=DIRECTION('center_axis',(0.,-1.,0.));
#1613=DIRECTION('ref_axis',(1.,0.,0.));
#1614=DIRECTION('center_axis',(0.,-1.,0.));
#1615=DIRECTION('ref_axis',(1.,0.,0.));
#1616=DIRECTION('',(0.,1.,0.));
#1617=DIRECTION('center_axis',(0.,-1.,0.));
#1618=DIRECTION('ref_axis',(1.,0.,0.));
#1619=DIRECTION('center_axis',(0.,1.,0.));
#1620=DIRECTION('ref_axis',(1.,0.,0.));
#1621=DIRECTION('axis',(0.,0.,1.));
#1622=DIRECTION('refdir',(1.,0.,0.));
#1623=DIRECTION('center_axis',(0.,-1.,0.));
#1624=DIRECTION('ref_axis',(1.,0.,0.));
#1625=DIRECTION('center_axis',(0.,-1.,0.));
#1626=DIRECTION('ref_axis',(1.,0.,0.));
#1627=DIRECTION('center_axis',(0.,-1.,0.));
#1628=DIRECTION('ref_axis',(1.,0.,0.));
#1629=DIRECTION('',(0.,1.,0.));
#1630=DIRECTION('center_axis',(0.,-1.,0.));
#1631=DIRECTION('ref_axis',(1.,0.,0.));
#1632=DIRECTION('center_axis',(0.,1.,0.));
#1633=DIRECTION('ref_axis',(0.,0.,1.));
#1634=DIRECTION('axis',(0.,0.,1.));
#1635=DIRECTION('refdir',(1.,0.,0.));
#1636=DIRECTION('center_axis',(0.,-1.,0.));
#1637=DIRECTION('ref_axis',(1.,0.,0.));
#1638=DIRECTION('center_axis',(0.,-1.,0.));
#1639=DIRECTION('ref_axis',(1.,0.,0.));
#1640=DIRECTION('',(0.,-1.,0.));
#1641=DIRECTION('center_axis',(0.,1.,0.));
#1642=DIRECTION('ref_axis',(1.,0.,0.));
#1643=DIRECTION('center_axis',(0.,-1.,0.));
#1644=DIRECTION('ref_axis',(1.,0.,0.));
#1645=DIRECTION('center_axis',(0.,-1.,0.));
#1646=DIRECTION('ref_axis',(1.,0.,0.));
#1647=DIRECTION('',(0.,-1.,0.));
#1648=DIRECTION('center_axis',(0.,-1.,0.));
#1649=DIRECTION('ref_axis',(1.,0.,0.));
#1650=DIRECTION('center_axis',(0.,1.,0.));
#1651=DIRECTION('ref_axis',(0.,0.,1.));
#1652=DIRECTION('',(-1.,0.,0.));
#1653=DIRECTION('',(0.,0.,-1.));
#1654=DIRECTION('',(1.,0.,0.));
#1655=DIRECTION('',(0.,0.,1.));
#1656=DIRECTION('center_axis',(1.,0.,0.));
#1657=DIRECTION('ref_axis',(0.,0.,-1.));
#1658=DIRECTION('',(0.,1.,0.));
#1659=DIRECTION('',(0.,0.,-1.));
#1660=DIRECTION('',(0.,1.,0.));
#1661=DIRECTION('center_axis',(0.,0.,-1.));
#1662=DIRECTION('ref_axis',(-1.,0.,0.));
#1663=DIRECTION('',(0.,1.,0.));
#1664=DIRECTION('',(-1.,0.,0.));
#1665=DIRECTION('center_axis',(0.,0.,1.));
#1666=DIRECTION('ref_axis',(1.,0.,0.));
#1667=DIRECTION('',(1.,0.,0.));
#1668=DIRECTION('',(0.,1.,0.));
#1669=DIRECTION('center_axis',(-1.,0.,0.));
#1670=DIRECTION('ref_axis',(0.,0.,1.));
#1671=DIRECTION('',(0.,0.,1.));
#1672=DIRECTION('center_axis',(0.,1.,0.));
#1673=DIRECTION('ref_axis',(0.,0.,1.));
#1674=DIRECTION('axis',(0.,0.,1.));
#1675=DIRECTION('refdir',(1.,0.,0.));
#1676=DIRECTION('center_axis',(0.983844577872192,0.,-0.179024709443944));
#1677=DIRECTION('ref_axis',(-0.179024709443944,0.,-0.983844577872192));
#1678=DIRECTION('',(-0.179024709443944,0.,-0.983844577872192));
#1679=DIRECTION('',(0.,1.,0.));
#1680=DIRECTION('',(-0.179024709443944,0.,-0.983844577872192));
#1681=DIRECTION('',(0.,1.,0.));
#1682=DIRECTION('center_axis',(-0.00140955899906737,0.,-0.999999006571221));
#1683=DIRECTION('ref_axis',(-0.999999006571221,0.,0.00140955899906737));
#1684=DIRECTION('',(0.999999006571221,0.,-0.00140955899906737));
#1685=DIRECTION('',(0.,1.,0.));
#1686=DIRECTION('',(0.999999006571221,0.,-0.00140955899906737));
#1687=DIRECTION('',(0.,1.,0.));
#1688=DIRECTION('center_axis',(0.,1.,0.));
#1689=DIRECTION('ref_axis',(1.,0.,0.));
#1690=DIRECTION('',(0.983844577872192,0.,0.179024709443943));
#1691=DIRECTION('center_axis',(0.,1.,0.));
#1692=DIRECTION('ref_axis',(1.,0.,0.));
#1693=DIRECTION('',(1.,0.,0.));
#1694=DIRECTION('center_axis',(0.,-1.,0.));
#1695=DIRECTION('ref_axis',(-1.,0.,0.));
#1696=DIRECTION('center_axis',(0.,-1.,0.));
#1697=DIRECTION('ref_axis',(1.,0.,0.));
#1698=DIRECTION('center_axis',(0.,-1.,0.));
#1699=DIRECTION('ref_axis',(1.,0.,0.));
#1700=DIRECTION('center_axis',(-0.179024709443943,0.,0.983844577872192));
#1701=DIRECTION('ref_axis',(0.983844577872192,0.,0.179024709443943));
#1702=DIRECTION('',(0.983844577872192,0.,0.179024709443943));
#1703=DIRECTION('',(0.,1.,0.));
#1704=DIRECTION('center_axis',(0.,1.,0.));
#1705=DIRECTION('ref_axis',(1.,0.,0.));
#1706=DIRECTION('center_axis',(0.,1.,0.));
#1707=DIRECTION('ref_axis',(1.,0.,0.));
#1708=DIRECTION('center_axis',(0.,-1.,0.));
#1709=DIRECTION('ref_axis',(1.,0.,0.));
#1710=DIRECTION('',(0.,-1.,0.));
#1711=DIRECTION('center_axis',(0.,1.,0.));
#1712=DIRECTION('ref_axis',(1.,0.,0.));
#1713=DIRECTION('center_axis',(0.,0.,1.));
#1714=DIRECTION('ref_axis',(1.,0.,0.));
#1715=DIRECTION('',(1.,0.,0.));
#1716=DIRECTION('',(0.,-1.,0.));
#1717=DIRECTION('center_axis',(0.,1.,0.));
#1718=DIRECTION('ref_axis',(1.,0.,0.));
#1719=DIRECTION('',(0.,-1.,0.));
#1720=DIRECTION('center_axis',(0.,-1.,0.));
#1721=DIRECTION('ref_axis',(1.,0.,0.));
#1722=DIRECTION('center_axis',(0.,1.,0.));
#1723=DIRECTION('ref_axis',(1.,0.,0.));
#1724=DIRECTION('center_axis',(0.,1.,0.));
#1725=DIRECTION('ref_axis',(-1.,0.,0.));
#1726=DIRECTION('center_axis',(0.,1.,0.));
#1727=DIRECTION('ref_axis',(-1.,0.,0.));
#1728=DIRECTION('axis',(0.,0.,1.));
#1729=DIRECTION('refdir',(1.,0.,0.));
#1730=DIRECTION('center_axis',(-1.,0.,0.));
#1731=DIRECTION('ref_axis',(0.,0.,1.));
#1732=DIRECTION('',(0.,-1.,0.));
#1733=DIRECTION('',(0.,0.,-1.));
#1734=DIRECTION('',(0.,1.,0.));
#1735=DIRECTION('',(0.,0.,1.));
#1736=DIRECTION('',(0.,1.,0.));
#1737=DIRECTION('center_axis',(0.,1.,0.));
#1738=DIRECTION('ref_axis',(1.,0.,0.));
#1739=DIRECTION('center_axis',(0.,-1.,0.));
#1740=DIRECTION('ref_axis',(-1.,0.,0.));
#1741=DIRECTION('',(1.,0.,0.));
#1742=DIRECTION('center_axis',(0.,1.,0.));
#1743=DIRECTION('ref_axis',(1.,0.,0.));
#1744=DIRECTION('center_axis',(0.,1.,0.));
#1745=DIRECTION('ref_axis',(-1.,0.,0.));
#1746=DIRECTION('center_axis',(0.,1.,0.));
#1747=DIRECTION('ref_axis',(-1.,0.,0.));
#1748=DIRECTION('',(0.,-1.,0.));
#1749=DIRECTION('center_axis',(0.,1.,0.));
#1750=DIRECTION('ref_axis',(-0.707106781186548,0.,-0.707106781186547));
#1751=DIRECTION('',(0.,-1.,0.));
#1752=DIRECTION('center_axis',(0.,-1.,0.));
#1753=DIRECTION('ref_axis',(1.,0.,0.));
#1754=DIRECTION('center_axis',(0.983844577872192,0.,-0.179024709443944));
#1755=DIRECTION('ref_axis',(-0.179024709443944,0.,-0.983844577872192));
#1756=DIRECTION('',(-0.179024709443944,0.,-0.983844577872192));
#1757=DIRECTION('',(0.,1.,0.));
#1758=DIRECTION('',(0.179024709443944,0.,0.983844577872192));
#1759=DIRECTION('',(0.,1.,0.));
#1760=DIRECTION('center_axis',(0.,1.,0.));
#1761=DIRECTION('ref_axis',(1.,0.,0.));
#1762=DIRECTION('',(-0.999999006571221,0.,0.00140955899906737));
#1763=DIRECTION('',(-1.,0.,0.));
#1764=DIRECTION('center_axis',(0.,1.,0.));
#1765=DIRECTION('ref_axis',(3.37710425741493E-16,0.,-1.));
#1766=DIRECTION('center_axis',(0.,1.,0.));
#1767=DIRECTION('ref_axis',(1.,0.,0.));
#1768=DIRECTION('center_axis',(0.,1.,0.));
#1769=DIRECTION('ref_axis',(3.37710425741493E-16,0.,-1.));
#1770=DIRECTION('',(0.,-1.,0.));
#1771=DIRECTION('center_axis',(0.,1.,0.));
#1772=DIRECTION('ref_axis',(3.37710425741493E-16,0.,-1.));
#1773=DIRECTION('center_axis',(0.,1.,0.));
#1774=DIRECTION('ref_axis',(1.,0.,0.));
#1775=DIRECTION('center_axis',(0.,-1.,0.));
#1776=DIRECTION('ref_axis',(1.,0.,0.));
#1777=DIRECTION('',(0.,-1.,0.));
#1778=DIRECTION('center_axis',(0.,0.,1.));
#1779=DIRECTION('ref_axis',(1.,0.,0.));
#1780=DIRECTION('',(1.,0.,0.));
#1781=DIRECTION('center_axis',(-0.00140955899906737,0.,-0.999999006571221));
#1782=DIRECTION('ref_axis',(-0.999999006571221,0.,0.00140955899906737));
#1783=DIRECTION('',(0.999999006571221,0.,-0.00140955899906737));
#1784=DIRECTION('center_axis',(0.,1.,0.));
#1785=DIRECTION('ref_axis',(0.,0.,1.));
#1786=DIRECTION('axis',(0.,0.,1.));
#1787=DIRECTION('refdir',(1.,0.,0.));
#1788=DIRECTION('center_axis',(0.,-1.,0.));
#1789=DIRECTION('ref_axis',(1.,0.,0.));
#1790=DIRECTION('center_axis',(0.,-1.,0.));
#1791=DIRECTION('ref_axis',(1.,0.,0.));
#1792=DIRECTION('center_axis',(0.,-1.,0.));
#1793=DIRECTION('ref_axis',(1.,0.,0.));
#1794=DIRECTION('',(0.,1.,0.));
#1795=DIRECTION('center_axis',(0.,-1.,0.));
#1796=DIRECTION('ref_axis',(1.,0.,0.));
#1797=DIRECTION('center_axis',(0.,1.,0.));
#1798=DIRECTION('ref_axis',(0.,0.,1.));
#1799=DIRECTION('axis',(0.,0.,1.));
#1800=DIRECTION('refdir',(1.,0.,0.));
#1801=DIRECTION('center_axis',(0.,-1.,0.));
#1802=DIRECTION('ref_axis',(1.,0.,0.));
#1803=DIRECTION('center_axis',(0.,-1.,0.));
#1804=DIRECTION('ref_axis',(1.,0.,0.));
#1805=DIRECTION('center_axis',(0.,1.,0.));
#1806=DIRECTION('ref_axis',(1.,0.,0.));
#1807=DIRECTION('center_axis',(0.,-1.,0.));
#1808=DIRECTION('ref_axis',(1.,0.,0.));
#1809=DIRECTION('',(0.,1.,0.));
#1810=DIRECTION('center_axis',(0.,1.,0.));
#1811=DIRECTION('ref_axis',(1.,0.,0.));
#1812=DIRECTION('center_axis',(0.,-1.,0.));
#1813=DIRECTION('ref_axis',(1.,0.,0.));
#1814=DIRECTION('center_axis',(0.,-1.,0.));
#1815=DIRECTION('ref_axis',(1.,0.,0.));
#1816=DIRECTION('',(0.,-1.,0.));
#1817=DIRECTION('center_axis',(0.,1.,0.));
#1818=DIRECTION('ref_axis',(0.,0.,1.));
#1819=DIRECTION('',(0.,0.,1.));
#1820=DIRECTION('',(1.,0.,0.));
#1821=DIRECTION('',(0.,0.,1.));
#1822=DIRECTION('',(1.,0.,0.));
#1823=DIRECTION('',(0.,0.,1.));
#1824=DIRECTION('',(1.,0.,0.));
#1825=DIRECTION('',(0.,0.,1.));
#1826=DIRECTION('',(1.,0.,0.));
#1827=DIRECTION('',(0.,0.,1.));
#1828=DIRECTION('',(1.,0.,0.));
#1829=DIRECTION('',(0.,0.,1.));
#1830=DIRECTION('',(1.,0.,0.));
#1831=DIRECTION('',(0.,0.,1.));
#1832=DIRECTION('',(1.,0.,0.));
#1833=DIRECTION('',(0.,0.,1.));
#1834=DIRECTION('',(1.,0.,0.));
#1835=CARTESIAN_POINT('',(0.,0.,0.));
#1836=CARTESIAN_POINT('',(0.,0.,0.));
#1837=CARTESIAN_POINT('Origin',(7.75064923678082,0.,83.4550501631985));
#1838=CARTESIAN_POINT('',(7.7506492069785,0.,83.4550501333962));
#1839=CARTESIAN_POINT('',(21.0224285630747,0.,96.7268294894923));
#1840=CARTESIAN_POINT('',(7.75064923678082,0.,83.4550501631985));
#1841=CARTESIAN_POINT('',(21.0224285630747,-5.,96.7268294894923));
#1842=CARTESIAN_POINT('',(21.0224285630747,0.,96.7268294894923));
#1843=CARTESIAN_POINT('',(7.7506492069785,-5.,83.4550501333962));
#1844=CARTESIAN_POINT('',(7.75064923678082,-5.,83.4550501631985));
#1845=CARTESIAN_POINT('',(7.7506492069785,0.,83.4550501333962));
#1846=CARTESIAN_POINT('Origin',(9.16486279915392,0.,82.0408366008254));
#1847=CARTESIAN_POINT('',(10.579076361527,0.,80.6266230384523));
#1848=CARTESIAN_POINT('Origin',(9.16486279915392,0.,82.0408366008254));
#1849=CARTESIAN_POINT('',(10.579076361527,-5.,80.6266230384523));
#1850=CARTESIAN_POINT('Origin',(9.16486279915392,-5.,82.0408366008254));
#1851=CARTESIAN_POINT('',(10.579076361527,0.,80.6266230384523));
#1852=CARTESIAN_POINT('Origin',(23.8508556878209,0.,93.8984023647461));
#1853=CARTESIAN_POINT('',(23.8508556878209,0.,93.8984023647461));
#1854=CARTESIAN_POINT('',(25.6442326956396,0.,95.6917793725649));
#1855=CARTESIAN_POINT('',(23.8508556878209,-5.,93.8984023647461));
#1856=CARTESIAN_POINT('',(25.6442326956396,-5.,95.6917793725649));
#1857=CARTESIAN_POINT('',(23.8508556878209,0.,93.8984023647461));
#1858=CARTESIAN_POINT('Origin',(27.1472176868794,0.,90.6020403656876));
#1859=CARTESIAN_POINT('',(27.1472176868794,0.,90.6020403656876));
#1860=CARTESIAN_POINT('',(17.7260665640161,0.,100.023191488551));
#1861=CARTESIAN_POINT('',(27.1472176868794,-5.,90.6020403656876));
#1862=CARTESIAN_POINT('',(17.7260665640161,-5.,100.023191488551));
#1863=CARTESIAN_POINT('',(27.1472176868794,0.,90.6020403656876));
#1864=CARTESIAN_POINT('Origin',(21.0224285630747,0.,96.7268294894923));
#1865=CARTESIAN_POINT('',(17.7260665640161,0.,100.023191488551));
#1866=CARTESIAN_POINT('',(17.7260665640161,0.,100.023191488551));
#1867=CARTESIAN_POINT('',(17.7260665640161,-5.,100.023191488551));
#1868=CARTESIAN_POINT('',(17.7260665640161,0.,100.023191488551));
#1869=CARTESIAN_POINT('',(17.7260665640161,-5.,100.023191488551));
#1870=CARTESIAN_POINT('Origin',(7.75064923678082,0.,62.2968974401444));
#1871=CARTESIAN_POINT('',(7.7506492069785,0.,62.2968974699467));
#1872=CARTESIAN_POINT('',(21.0224285630747,0.,49.0251181138506));
#1873=CARTESIAN_POINT('',(7.75064923678082,0.,62.2968974401444));
#1874=CARTESIAN_POINT('',(7.7506492069785,-5.,62.2968974699467));
#1875=CARTESIAN_POINT('',(7.7506492069785,0.,62.2968974699467));
#1876=CARTESIAN_POINT('',(21.0224285630747,-5.,49.0251181138506));
#1877=CARTESIAN_POINT('',(7.75064923678082,-5.,62.2968974401444));
#1878=CARTESIAN_POINT('',(21.0224285630747,0.,49.0251181138506));
#1879=CARTESIAN_POINT('Origin',(9.16486279915392,0.,63.7111110025175));
#1880=CARTESIAN_POINT('',(10.579076361527,0.,65.1253245648906));
#1881=CARTESIAN_POINT('Origin',(9.16486279915392,0.,63.7111110025175));
#1882=CARTESIAN_POINT('',(10.579076361527,-5.,65.1253245648906));
#1883=CARTESIAN_POINT('',(10.579076361527,0.,65.1253245648906));
#1884=CARTESIAN_POINT('Origin',(9.16486279915392,-5.,63.7111110025175));
#1885=CARTESIAN_POINT('Origin',(23.8508556878209,0.,51.8535452385968));
#1886=CARTESIAN_POINT('',(23.8508556878209,0.,51.8535452385968));
#1887=CARTESIAN_POINT('',(25.6442326956396,0.,50.060168230778));
#1888=CARTESIAN_POINT('',(23.8508556878209,-5.,51.8535452385968));
#1889=CARTESIAN_POINT('',(23.8508556878209,0.,51.8535452385968));
#1890=CARTESIAN_POINT('',(25.6442326956396,-5.,50.060168230778));
#1891=CARTESIAN_POINT('Origin',(27.1472176868794,0.,55.1499072376553));
#1892=CARTESIAN_POINT('',(27.1472176868794,0.,55.1499072376553));
#1893=CARTESIAN_POINT('',(17.7260665640161,0.,45.728756114792));
#1894=CARTESIAN_POINT('',(27.1472176868794,-5.,55.1499072376553));
#1895=CARTESIAN_POINT('',(27.1472176868794,0.,55.1499072376553));
#1896=CARTESIAN_POINT('',(17.7260665640161,-5.,45.728756114792));
#1897=CARTESIAN_POINT('Origin',(46.5759738016714,0.,72.8759738016714));
#1898=CARTESIAN_POINT('Origin',(46.5759738016714,0.,72.8759738016714));
#1899=CARTESIAN_POINT('Origin',(46.5759738016714,-5.,72.8759738016714));
#1900=CARTESIAN_POINT('Origin',(21.0224285630747,0.,49.0251181138506));
#1901=CARTESIAN_POINT('',(17.7260665640161,0.,45.728756114792));
#1902=CARTESIAN_POINT('',(17.7260665640161,0.,45.728756114792));
#1903=CARTESIAN_POINT('',(17.7260665640161,-5.,45.728756114792));
#1904=CARTESIAN_POINT('',(17.7260665640161,-5.,45.728756114792));
#1905=CARTESIAN_POINT('',(17.7260665640161,0.,45.728756114792));
#1906=CARTESIAN_POINT('Origin',(-7.75064923678082,0.,83.4550501631985));
#1907=CARTESIAN_POINT('',(-7.7506492069785,0.,83.4550501333962));
#1908=CARTESIAN_POINT('',(-21.0224285630747,0.,96.7268294894923));
#1909=CARTESIAN_POINT('',(-7.75064923678082,0.,83.4550501631985));
#1910=CARTESIAN_POINT('',(-7.7506492069785,-5.,83.4550501333962));
#1911=CARTESIAN_POINT('',(-7.7506492069785,0.,83.4550501333962));
#1912=CARTESIAN_POINT('',(-21.0224285630747,-5.,96.7268294894923));
#1913=CARTESIAN_POINT('',(-7.75064923678082,-5.,83.4550501631985));
#1914=CARTESIAN_POINT('',(-21.0224285630747,0.,96.7268294894923));
#1915=CARTESIAN_POINT('Origin',(-9.16486279915392,0.,82.0408366008254));
#1916=CARTESIAN_POINT('',(-10.579076361527,0.,80.6266230384523));
#1917=CARTESIAN_POINT('Origin',(-9.16486279915392,0.,82.0408366008254));
#1918=CARTESIAN_POINT('',(-10.579076361527,-5.,80.6266230384523));
#1919=CARTESIAN_POINT('',(-10.579076361527,0.,80.6266230384523));
#1920=CARTESIAN_POINT('Origin',(-9.16486279915392,-5.,82.0408366008254));
#1921=CARTESIAN_POINT('Origin',(-23.8508556878209,0.,93.8984023647461));
#1922=CARTESIAN_POINT('',(-23.8508556878209,0.,93.8984023647461));
#1923=CARTESIAN_POINT('',(-25.6442326956396,0.,95.6917793725649));
#1924=CARTESIAN_POINT('',(-23.8508556878209,-5.,93.8984023647461));
#1925=CARTESIAN_POINT('',(-23.8508556878209,0.,93.8984023647461));
#1926=CARTESIAN_POINT('',(-25.6442326956396,-5.,95.6917793725649));
#1927=CARTESIAN_POINT('Origin',(-27.1472176868794,0.,90.6020403656876));
#1928=CARTESIAN_POINT('',(-27.1472176868794,0.,90.6020403656876));
#1929=CARTESIAN_POINT('',(-17.7260665640161,0.,100.023191488551));
#1930=CARTESIAN_POINT('',(-27.1472176868794,-5.,90.6020403656876));
#1931=CARTESIAN_POINT('',(-27.1472176868794,0.,90.6020403656876));
#1932=CARTESIAN_POINT('',(-17.7260665640161,-5.,100.023191488551));
#1933=CARTESIAN_POINT('Origin',(0.,0.,119.451947603343));
#1934=CARTESIAN_POINT('',(-17.7260665640161,0.,100.023191488551));
#1935=CARTESIAN_POINT('Origin',(1.53080849893419E-15,0.,119.451947603343));
#1936=CARTESIAN_POINT('',(-17.7260665640161,-5.,100.023191488551));
#1937=CARTESIAN_POINT('',(-17.7260665640161,0.,100.023191488551));
#1938=CARTESIAN_POINT('Origin',(1.53080849893419E-15,-5.,119.451947603343));
#1939=CARTESIAN_POINT('Origin',(-21.0224285630747,0.,96.7268294894923));
#1940=CARTESIAN_POINT('',(-17.7260665640161,0.,100.023191488551));
#1941=CARTESIAN_POINT('',(-17.7260665640161,-5.,100.023191488551));
#1942=CARTESIAN_POINT('Origin',(-7.75064923678082,0.,62.2968974401444));
#1943=CARTESIAN_POINT('',(-7.7506492069785,0.,62.2968974699467));
#1944=CARTESIAN_POINT('',(-21.0224285630747,0.,49.0251181138506));
#1945=CARTESIAN_POINT('',(-7.75064923678082,0.,62.2968974401444));
#1946=CARTESIAN_POINT('',(-21.0224285630747,-5.,49.0251181138506));
#1947=CARTESIAN_POINT('',(-21.0224285630747,0.,49.0251181138506));
#1948=CARTESIAN_POINT('',(-7.7506492069785,-5.,62.2968974699467));
#1949=CARTESIAN_POINT('',(-7.75064923678082,-5.,62.2968974401444));
#1950=CARTESIAN_POINT('',(-7.7506492069785,0.,62.2968974699467));
#1951=CARTESIAN_POINT('Origin',(-9.16486279915392,0.,63.7111110025175));
#1952=CARTESIAN_POINT('',(-10.579076361527,0.,65.1253245648906));
#1953=CARTESIAN_POINT('Origin',(-9.16486279915392,0.,63.7111110025175));
#1954=CARTESIAN_POINT('',(-10.579076361527,-5.,65.1253245648906));
#1955=CARTESIAN_POINT('Origin',(-9.16486279915392,-5.,63.7111110025175));
#1956=CARTESIAN_POINT('',(-10.579076361527,0.,65.1253245648906));
#1957=CARTESIAN_POINT('Origin',(-23.8508556878209,0.,51.8535452385968));
#1958=CARTESIAN_POINT('',(-23.8508556878209,0.,51.8535452385968));
#1959=CARTESIAN_POINT('',(-25.6442326956396,0.,50.060168230778));
#1960=CARTESIAN_POINT('',(-23.8508556878209,-5.,51.8535452385968));
#1961=CARTESIAN_POINT('',(-25.6442326956396,-5.,50.060168230778));
#1962=CARTESIAN_POINT('',(-23.8508556878209,0.,51.8535452385968));
#1963=CARTESIAN_POINT('Origin',(-27.1472176868794,0.,55.1499072376553));
#1964=CARTESIAN_POINT('',(-27.1472176868794,0.,55.1499072376553));
#1965=CARTESIAN_POINT('',(-17.7260665640161,0.,45.728756114792));
#1966=CARTESIAN_POINT('',(-27.1472176868794,-5.,55.1499072376553));
#1967=CARTESIAN_POINT('',(-17.7260665640161,-5.,45.728756114792));
#1968=CARTESIAN_POINT('',(-27.1472176868794,0.,55.1499072376553));
#1969=CARTESIAN_POINT('Origin',(-46.5759738016714,0.,72.8759738016714));
#1970=CARTESIAN_POINT('Origin',(-46.5759738016714,0.,72.8759738016714));
#1971=CARTESIAN_POINT('Origin',(-46.5759738016714,-5.,72.8759738016714));
#1972=CARTESIAN_POINT('Origin',(0.,0.,72.8759738016714));
#1973=CARTESIAN_POINT('',(-2.5,-5.,72.8759738016714));
#1974=CARTESIAN_POINT('Origin',(1.53080849893419E-15,-5.,72.8759738016714));
#1975=CARTESIAN_POINT('',(-2.5,0.,72.8759738016714));
#1976=CARTESIAN_POINT('',(-2.5,0.,72.8759738016714));
#1977=CARTESIAN_POINT('Origin',(0.,0.,72.8759738016714));
#1978=CARTESIAN_POINT('Origin',(0.,0.,26.3));
#1979=CARTESIAN_POINT('',(-17.7260665640161,0.,45.728756114792));
#1980=CARTESIAN_POINT('Origin',(0.,0.,26.3));
#1981=CARTESIAN_POINT('',(-17.7260665640161,-5.,45.728756114792));
#1982=CARTESIAN_POINT('Origin',(0.,-5.,26.3));
#1983=CARTESIAN_POINT('',(-17.7260665640161,0.,45.728756114792));
#1984=CARTESIAN_POINT('Origin',(-21.0224285630747,0.,49.0251181138506));
#1985=CARTESIAN_POINT('',(-17.7260665640161,0.,45.728756114792));
#1986=CARTESIAN_POINT('',(-17.7260665640161,-5.,45.728756114792));
#1987=CARTESIAN_POINT('Origin',(-13.5736088434397,0.,59.3023649582317));
#1988=CARTESIAN_POINT('Origin',(-13.5736088434397,-5.,59.3023649582317));
#1989=CARTESIAN_POINT('',(0.,0.,0.));
#1990=CARTESIAN_POINT('Origin',(23.2879869008357,-5.,49.5879869008357));
#1991=CARTESIAN_POINT('',(21.5379869008357,-5.,49.5879869008357));
#1992=CARTESIAN_POINT('Origin',(23.2879869008357,-5.,49.5879869008357));
#1993=CARTESIAN_POINT('Origin',(23.2879869008357,0.,49.5879869008357));
#1994=CARTESIAN_POINT('',(21.5379869008357,3.,49.5879869008357));
#1995=CARTESIAN_POINT('',(21.5379869008357,0.,49.5879869008357));
#1996=CARTESIAN_POINT('Origin',(23.2879869008357,3.,49.5879869008357));
#1997=CARTESIAN_POINT('Origin',(14.3033855617004,3.,40.6033855617004));
#1998=CARTESIAN_POINT('',(0.,0.,0.));
#1999=CARTESIAN_POINT('Origin',(1.66533453693773E-15,-5.,72.8759738016714));
#2000=CARTESIAN_POINT('',(-2.5,-5.,72.8759738016714));
#2001=CARTESIAN_POINT('Origin',(1.53080849893419E-15,-5.,72.8759738016714));
#2002=CARTESIAN_POINT('Origin',(1.53080849893419E-15,3.,72.8759738016714));
#2003=CARTESIAN_POINT('',(-2.5,5.,72.8759738016714));
#2004=CARTESIAN_POINT('',(-2.5,3.,72.8759738016714));
#2005=CARTESIAN_POINT('Origin',(1.53080849893419E-15,5.,72.8759738016714));
#2006=CARTESIAN_POINT('Origin',(0.,5.,50.));
#2007=CARTESIAN_POINT('',(0.,0.,0.));
#2008=CARTESIAN_POINT('Origin',(0.,3.,26.3));
#2009=CARTESIAN_POINT('',(-2.5,5.,26.3));
#2010=CARTESIAN_POINT('Origin',(0.,5.,26.3));
#2011=CARTESIAN_POINT('',(-2.5,3.,26.3));
#2012=CARTESIAN_POINT('',(-2.5,3.,26.3));
#2013=CARTESIAN_POINT('Origin',(0.,3.,26.3));
#2014=CARTESIAN_POINT('Origin',(1.53080849893419E-15,3.,72.8759738016714));
#2015=CARTESIAN_POINT('',(-2.5,5.,72.8759738016714));
#2016=CARTESIAN_POINT('Origin',(1.53080849893419E-15,5.,72.8759738016714));
#2017=CARTESIAN_POINT('',(-2.5,3.,72.8759738016714));
#2018=CARTESIAN_POINT('',(-2.5,3.,72.8759738016714));
#2019=CARTESIAN_POINT('Origin',(1.53080849893419E-15,3.,72.8759738016714));
#2020=CARTESIAN_POINT('Origin',(0.,3.,50.));
#2021=CARTESIAN_POINT('',(38.,3.,-10.));
#2022=CARTESIAN_POINT('',(-38.,3.,-10.));
#2023=CARTESIAN_POINT('',(19.,3.,-10.));
#2024=CARTESIAN_POINT('',(38.,3.,110.));
#2025=CARTESIAN_POINT('',(38.,3.,80.));
#2026=CARTESIAN_POINT('',(-38.,3.,110.));
#2027=CARTESIAN_POINT('',(-19.,3.,110.));
#2028=CARTESIAN_POINT('',(-38.,3.,20.));
#2029=CARTESIAN_POINT('Origin',(38.,0.,110.));
#2030=CARTESIAN_POINT('',(38.,5.,-10.));
#2031=CARTESIAN_POINT('',(38.,0.,-10.));
#2032=CARTESIAN_POINT('',(38.,5.,110.));
#2033=CARTESIAN_POINT('',(38.,5.,-10.));
#2034=CARTESIAN_POINT('',(38.,0.,110.));
#2035=CARTESIAN_POINT('Origin',(38.,0.,-10.));
#2036=CARTESIAN_POINT('',(-38.,5.,-10.));
#2037=CARTESIAN_POINT('',(-38.,0.,-10.));
#2038=CARTESIAN_POINT('',(0.,5.,-10.));
#2039=CARTESIAN_POINT('Origin',(-38.,0.,110.));
#2040=CARTESIAN_POINT('',(-38.,5.,110.));
#2041=CARTESIAN_POINT('',(-38.,5.,110.));
#2042=CARTESIAN_POINT('',(-38.,0.,110.));
#2043=CARTESIAN_POINT('Origin',(-38.,0.,-10.));
#2044=CARTESIAN_POINT('',(-38.,5.,-10.));
#2045=CARTESIAN_POINT('Origin',(0.,5.,50.));
#2046=CARTESIAN_POINT('',(0.,0.,0.));
#2047=CARTESIAN_POINT('Origin',(27.8026817657391,0.,45.0732920359323));
#2048=CARTESIAN_POINT('',(28.4531709343409,0.,48.6481071744755));
#2049=CARTESIAN_POINT('',(24.3866105410464,0.,26.3));
#2050=CARTESIAN_POINT('',(25.9192569340967,0.,34.7227805663332));
#2051=CARTESIAN_POINT('',(24.3866105410464,3.,26.3));
#2052=CARTESIAN_POINT('',(24.3866105410464,0.,26.3));
#2053=CARTESIAN_POINT('',(28.4531709343409,3.,48.6481071744755));
#2054=CARTESIAN_POINT('',(24.3866105410464,3.,26.3));
#2055=CARTESIAN_POINT('',(28.4531709346647,0.,48.648107176255));
#2056=CARTESIAN_POINT('Origin',(0.0687842225651092,-5.,50.6991268223128));
#2057=CARTESIAN_POINT('',(0.,0.,50.699223777829));
#2058=CARTESIAN_POINT('',(0.0687842225651092,0.,50.6991268223128));
#2059=CARTESIAN_POINT('',(1.08481843563973,0.,50.6976946607217));
#2060=CARTESIAN_POINT('',(0.0687842225651103,3.,50.6991268223128));
#2061=CARTESIAN_POINT('',(0.0687842225651292,3.,50.6991268223128));
#2062=CARTESIAN_POINT('',(0.,3.,50.699223777829));
#2063=CARTESIAN_POINT('',(7.19318601548171,3.,50.6890845476763));
#2064=CARTESIAN_POINT('',(0.,3.,50.699223777829));
#2065=CARTESIAN_POINT('Origin',(14.3033855617004,3.,40.6033855617004));
#2066=CARTESIAN_POINT('',(22.3481071813648,3.,54.7531709355945));
#2067=CARTESIAN_POINT('',(4.44089209850063E-15,3.,50.6866105410464));
#2068=CARTESIAN_POINT('Origin',(23.2879869008357,3.,49.5879869008357));
#2069=CARTESIAN_POINT('',(24.399223777829,3.,26.3));
#2070=CARTESIAN_POINT('',(0.,3.,26.3));
#2071=CARTESIAN_POINT('Origin',(0.,3.,26.3));
#2072=CARTESIAN_POINT('',(-2.5,3.,26.3));
#2073=CARTESIAN_POINT('Origin',(0.,3.,26.3));
#2074=CARTESIAN_POINT('',(21.5379869008357,3.,49.5879869008357));
#2075=CARTESIAN_POINT('Origin',(23.2879869008357,3.,49.5879869008357));
#2076=CARTESIAN_POINT('Origin',(0.0687842225651098,0.,50.6991268223128));
#2077=CARTESIAN_POINT('',(22.3481071813648,0.,54.7531709355945));
#2078=CARTESIAN_POINT('',(4.44089209850063E-15,0.,50.6866105410464));
#2079=CARTESIAN_POINT('',(22.3481071813648,0.,54.7531709355945));
#2080=CARTESIAN_POINT('Origin',(23.2879869008357,0.,49.5879869008357));
#2081=CARTESIAN_POINT('Origin',(23.2879869008357,0.,49.5879869008357));
#2082=CARTESIAN_POINT('Origin',(23.2879869008357,0.,49.5879869008357));
#2083=CARTESIAN_POINT('',(21.5379869008357,0.,49.5879869008357));
#2084=CARTESIAN_POINT('',(21.5379869008357,0.,49.5879869008357));
#2085=CARTESIAN_POINT('Origin',(23.2879869008357,0.,49.5879869008357));
#2086=CARTESIAN_POINT('Origin',(24.3866105410464,0.,26.3));
#2087=CARTESIAN_POINT('',(24.399223777829,0.,26.3));
#2088=CARTESIAN_POINT('',(13.2279960512749,0.,26.3));
#2089=CARTESIAN_POINT('',(24.399223777829,3.,26.3));
#2090=CARTESIAN_POINT('Origin',(0.,0.,26.3));
#2091=CARTESIAN_POINT('',(-2.5,0.,26.3));
#2092=CARTESIAN_POINT('',(-2.5,0.,26.3));
#2093=CARTESIAN_POINT('Origin',(0.,0.,26.3));
#2094=CARTESIAN_POINT('Origin',(14.3033855617004,0.,40.6033855617004));
#2095=CARTESIAN_POINT('Origin',(0.,0.,26.3));
#2096=CARTESIAN_POINT('Origin',(0.,3.,26.3));
#2097=CARTESIAN_POINT('',(0.,0.,0.));
#2098=CARTESIAN_POINT('Origin',(0.,3.,26.3));
#2099=CARTESIAN_POINT('',(0.,3.,50.699223777829));
#2100=CARTESIAN_POINT('',(0.,0.,50.699223777829));
#2101=CARTESIAN_POINT('',(0.,3.,50.699223777829));
#2102=CARTESIAN_POINT('',(4.16333634234434E-15,3.,52.6));
#2103=CARTESIAN_POINT('',(0.,3.,33.4516927808502));
#2104=CARTESIAN_POINT('',(4.16333634234434E-15,-5.,52.6));
#2105=CARTESIAN_POINT('',(4.44089209850063E-15,0.,52.6));
#2106=CARTESIAN_POINT('',(0.,-5.,50.699223777829));
#2107=CARTESIAN_POINT('',(0.,-5.,26.3));
#2108=CARTESIAN_POINT('',(0.,3.,50.699223777829));
#2109=CARTESIAN_POINT('Origin',(14.3033855617004,3.,40.6033855617004));
#2110=CARTESIAN_POINT('',(24.399223777829,3.,26.3));
#2111=CARTESIAN_POINT('Origin',(0.,3.,26.3));
#2112=CARTESIAN_POINT('',(26.3,3.,26.3));
#2113=CARTESIAN_POINT('',(0.,3.,26.3));
#2114=CARTESIAN_POINT('Origin',(0.,3.,26.3));
#2115=CARTESIAN_POINT('Origin',(0.,3.,26.3));
#2116=CARTESIAN_POINT('',(24.399223777829,0.,26.3));
#2117=CARTESIAN_POINT('Origin',(0.,0.,26.3));
#2118=CARTESIAN_POINT('',(24.399223777829,3.,26.3));
#2119=CARTESIAN_POINT('Origin',(0.,0.,26.3));
#2120=CARTESIAN_POINT('',(26.3,-5.,26.3));
#2121=CARTESIAN_POINT('',(26.3,0.,26.3));
#2122=CARTESIAN_POINT('Origin',(0.,-5.,26.3));
#2123=CARTESIAN_POINT('Origin',(27.8026817657391,0.,45.0732920359323));
#2124=CARTESIAN_POINT('',(24.3991268223128,0.,26.3687842225651));
#2125=CARTESIAN_POINT('',(24.3866105410464,0.,26.3));
#2126=CARTESIAN_POINT('',(25.9192569340967,0.,34.7227805663332));
#2127=CARTESIAN_POINT('',(24.3991268223128,-5.,26.3687842225651));
#2128=CARTESIAN_POINT('',(24.3991268223128,0.,26.3687842225651));
#2129=CARTESIAN_POINT('',(24.3866105410464,-5.,26.3));
#2130=CARTESIAN_POINT('',(24.3866105410464,-5.,26.3));
#2131=CARTESIAN_POINT('',(24.3866105410464,0.,26.3));
#2132=CARTESIAN_POINT('Origin',(0.,-5.,26.3));
#2133=CARTESIAN_POINT('',(0.0687842225651092,-5.,50.6991268223128));
#2134=CARTESIAN_POINT('',(0.0515881669226298,-5.,50.6991510611919));
#2135=CARTESIAN_POINT('',(0.,-5.,26.3));
#2136=CARTESIAN_POINT('Origin',(26.3,-5.,52.6));
#2137=CARTESIAN_POINT('',(-2.5,-5.,26.3));
#2138=CARTESIAN_POINT('Origin',(0.,-5.,26.3));
#2139=CARTESIAN_POINT('Origin',(26.3,0.,52.6));
#2140=CARTESIAN_POINT('',(0.0687842225651092,0.,50.6991268223128));
#2141=CARTESIAN_POINT('',(0.0687842225651059,0.,50.6991268223128));
#2142=CARTESIAN_POINT('Origin',(26.3,0.,52.6));
#2143=CARTESIAN_POINT('Origin',(0.,0.,26.3));
#2144=CARTESIAN_POINT('',(-2.5,0.,26.3));
#2145=CARTESIAN_POINT('Origin',(0.,0.,26.3));
#2146=CARTESIAN_POINT('',(-2.5,0.,26.3));
#2147=CARTESIAN_POINT('Origin',(24.3866105410464,0.,26.3));
#2148=CARTESIAN_POINT('',(13.2279960512749,0.,26.3));
#2149=CARTESIAN_POINT('Origin',(0.0687842225651092,-5.,50.6991268223128));
#2150=CARTESIAN_POINT('',(1.08481843563973,0.,50.6976946607217));
#2151=CARTESIAN_POINT('Origin',(2.06938156150334,0.,28.3693815615033));
#2152=CARTESIAN_POINT('',(0.,0.,0.));
#2153=CARTESIAN_POINT('Origin',(0.,-5.,26.3));
#2154=CARTESIAN_POINT('',(-2.5,-5.,26.3));
#2155=CARTESIAN_POINT('Origin',(0.,-5.,26.3));
#2156=CARTESIAN_POINT('Origin',(0.,3.,26.3));
#2157=CARTESIAN_POINT('',(-2.5,5.,26.3));
#2158=CARTESIAN_POINT('',(-2.5,3.,26.3));
#2159=CARTESIAN_POINT('Origin',(0.,5.,26.3));
#2160=CARTESIAN_POINT('Origin',(0.,5.,50.));
#2161=CARTESIAN_POINT('',(0.,0.,0.));
#2162=CARTESIAN_POINT('Origin',(1.66533453693773E-15,0.,72.8759738016714));
#2163=CARTESIAN_POINT('',(-4.5,0.,72.8759738016714));
#2164=CARTESIAN_POINT('Origin',(1.53080849893419E-15,0.,72.8759738016714));
#2165=CARTESIAN_POINT('',(-2.5,0.,72.8759738016714));
#2166=CARTESIAN_POINT('Origin',(1.53080849893419E-15,0.,72.8759738016714));
#2167=CARTESIAN_POINT('Origin',(1.53080849893419E-15,3.,72.8759738016714));
#2168=CARTESIAN_POINT('',(-4.5,3.,72.8759738016714));
#2169=CARTESIAN_POINT('',(-4.5,3.,72.8759738016714));
#2170=CARTESIAN_POINT('Origin',(1.53080849893419E-15,3.,72.8759738016714));
#2171=CARTESIAN_POINT('Origin',(1.53080849893419E-15,3.,72.8759738016714));
#2172=CARTESIAN_POINT('',(-2.5,3.,72.8759738016714));
#2173=CARTESIAN_POINT('Origin',(1.53080849893419E-15,3.,72.8759738016714));
#2174=CARTESIAN_POINT('',(-2.5,3.,72.8759738016714));
#2175=CARTESIAN_POINT('Origin',(0.,3.,50.));
#2176=CARTESIAN_POINT('',(0.,0.,0.));
#2177=CARTESIAN_POINT('',(0.,0.,0.));
#2178=CARTESIAN_POINT('',(0.,0.,0.));
#2179=CARTESIAN_POINT('',(0.,0.,0.));
#2180=CARTESIAN_POINT('',(0.,0.,0.));
#2181=CARTESIAN_POINT('',(0.,0.,0.));
#2182=CARTESIAN_POINT('',(0.,0.,0.));
#2183=CARTESIAN_POINT('',(0.,0.,0.));
#2184=UNCERTAINTY_MEASURE_WITH_UNIT(LENGTH_MEASURE(0.01),#2204,
'DISTANCE_ACCURACY_VALUE',
'Maximum model space distance between geometric entities at asserted c
onnectivities');
#2185=UNCERTAINTY_MEASURE_WITH_UNIT(LENGTH_MEASURE(0.01),#2204,
'DISTANCE_ACCURACY_VALUE',
'Maximum model space distance between geometric entities at asserted c
onnectivities');
#2186=UNCERTAINTY_MEASURE_WITH_UNIT(LENGTH_MEASURE(0.01),#2204,
'DISTANCE_ACCURACY_VALUE',
'Maximum model space distance between geometric entities at asserted c
onnectivities');
#2187=UNCERTAINTY_MEASURE_WITH_UNIT(LENGTH_MEASURE(0.01),#2204,
'DISTANCE_ACCURACY_VALUE',
'Maximum model space distance between geometric entities at asserted c
onnectivities');
#2188=UNCERTAINTY_MEASURE_WITH_UNIT(LENGTH_MEASURE(0.01),#2204,
'DISTANCE_ACCURACY_VALUE',
'Maximum model space distance between geometric entities at asserted c
onnectivities');
#2189=UNCERTAINTY_MEASURE_WITH_UNIT(LENGTH_MEASURE(0.01),#2204,
'DISTANCE_ACCURACY_VALUE',
'Maximum model space distance between geometric entities at asserted c
onnectivities');
#2190=UNCERTAINTY_MEASURE_WITH_UNIT(LENGTH_MEASURE(0.01),#2204,
'DISTANCE_ACCURACY_VALUE',
'Maximum model space distance between geometric entities at asserted c
onnectivities');
#2191=UNCERTAINTY_MEASURE_WITH_UNIT(LENGTH_MEASURE(0.01),#2204,
'DISTANCE_ACCURACY_VALUE',
'Maximum model space distance between geometric entities at asserted c
onnectivities');
#2192=UNCERTAINTY_MEASURE_WITH_UNIT(LENGTH_MEASURE(0.01),#2204,
'DISTANCE_ACCURACY_VALUE',
'Maximum model space distance between geometric entities at asserted c
onnectivities');
#2193=UNCERTAINTY_MEASURE_WITH_UNIT(LENGTH_MEASURE(0.01),#2204,
'DISTANCE_ACCURACY_VALUE',
'Maximum model space distance between geometric entities at asserted c
onnectivities');
#2194=(
GEOMETRIC_REPRESENTATION_CONTEXT(3)
GLOBAL_UNCERTAINTY_ASSIGNED_CONTEXT((#2184))
GLOBAL_UNIT_ASSIGNED_CONTEXT((#2204,#2206,#2207))
REPRESENTATION_CONTEXT('','3D')
);
#2195=(
GEOMETRIC_REPRESENTATION_CONTEXT(3)
GLOBAL_UNCERTAINTY_ASSIGNED_CONTEXT((#2185))
GLOBAL_UNIT_ASSIGNED_CONTEXT((#2204,#2206,#2207))
REPRESENTATION_CONTEXT('','3D')
);
#2196=(
GEOMETRIC_REPRESENTATION_CONTEXT(3)
GLOBAL_UNCERTAINTY_ASSIGNED_CONTEXT((#2186))
GLOBAL_UNIT_ASSIGNED_CONTEXT((#2204,#2206,#2207))
REPRESENTATION_CONTEXT('','3D')
);
#2197=(
GEOMETRIC_REPRESENTATION_CONTEXT(3)
GLOBAL_UNCERTAINTY_ASSIGNED_CONTEXT((#2187))
GLOBAL_UNIT_ASSIGNED_CONTEXT((#2204,#2206,#2207))
REPRESENTATION_CONTEXT('','3D')
);
#2198=(
GEOMETRIC_REPRESENTATION_CONTEXT(3)
GLOBAL_UNCERTAINTY_ASSIGNED_CONTEXT((#2188))
GLOBAL_UNIT_ASSIGNED_CONTEXT((#2204,#2206,#2207))
REPRESENTATION_CONTEXT('','3D')
);
#2199=(
GEOMETRIC_REPRESENTATION_CONTEXT(3)
GLOBAL_UNCERTAINTY_ASSIGNED_CONTEXT((#2189))
GLOBAL_UNIT_ASSIGNED_CONTEXT((#2204,#2206,#2207))
REPRESENTATION_CONTEXT('','3D')
);
#2200=(
GEOMETRIC_REPRESENTATION_CONTEXT(3)
GLOBAL_UNCERTAINTY_ASSIGNED_CONTEXT((#2190))
GLOBAL_UNIT_ASSIGNED_CONTEXT((#2204,#2206,#2207))
REPRESENTATION_CONTEXT('','3D')
);
#2201=(
GEOMETRIC_REPRESENTATION_CONTEXT(3)
GLOBAL_UNCERTAINTY_ASSIGNED_CONTEXT((#2191))
GLOBAL_UNIT_ASSIGNED_CONTEXT((#2204,#2206,#2207))
REPRESENTATION_CONTEXT('','3D')
);
#2202=(
GEOMETRIC_REPRESENTATION_CONTEXT(3)
GLOBAL_UNCERTAINTY_ASSIGNED_CONTEXT((#2192))
GLOBAL_UNIT_ASSIGNED_CONTEXT((#2204,#2206,#2207))
REPRESENTATION_CONTEXT('','3D')
);
#2203=(
GEOMETRIC_REPRESENTATION_CONTEXT(3)
GLOBAL_UNCERTAINTY_ASSIGNED_CONTEXT((#2193))
GLOBAL_UNIT_ASSIGNED_CONTEXT((#2204,#2206,#2207))
REPRESENTATION_CONTEXT('','3D')
);
#2204=(
LENGTH_UNIT()
NAMED_UNIT(*)
SI_UNIT(.MILLI.,.METRE.)
);
#2205=(
LENGTH_UNIT()
NAMED_UNIT(*)
SI_UNIT($,.METRE.)
);
#2206=(
NAMED_UNIT(*)
PLANE_ANGLE_UNIT()
SI_UNIT($,.RADIAN.)
);
#2207=(
NAMED_UNIT(*)
SI_UNIT($,.STERADIAN.)
SOLID_ANGLE_UNIT()
);
#2208=SHAPE_DEFINITION_REPRESENTATION(#2217,#2234);
#2209=SHAPE_DEFINITION_REPRESENTATION(#2218,#2235);
#2210=SHAPE_DEFINITION_REPRESENTATION(#2219,#2236);
#2211=SHAPE_DEFINITION_REPRESENTATION(#2220,#2237);
#2212=SHAPE_DEFINITION_REPRESENTATION(#2221,#2238);
#2213=SHAPE_DEFINITION_REPRESENTATION(#2222,#2239);
#2214=SHAPE_DEFINITION_REPRESENTATION(#2223,#2240);
#2215=SHAPE_DEFINITION_REPRESENTATION(#2224,#2241);
#2216=SHAPE_DEFINITION_REPRESENTATION(#2225,#2242);
#2217=PRODUCT_DEFINITION_SHAPE('',$,#2244);
#2218=PRODUCT_DEFINITION_SHAPE('',$,#2245);
#2219=PRODUCT_DEFINITION_SHAPE('',$,#2246);
#2220=PRODUCT_DEFINITION_SHAPE('',$,#2247);
#2221=PRODUCT_DEFINITION_SHAPE('',$,#2248);
#2222=PRODUCT_DEFINITION_SHAPE('',$,#2249);
#2223=PRODUCT_DEFINITION_SHAPE('',$,#2250);
#2224=PRODUCT_DEFINITION_SHAPE('',$,#2251);
#2225=PRODUCT_DEFINITION_SHAPE('',$,#2252);
#2226=PRODUCT_DEFINITION_SHAPE($,$,#35);
#2227=PRODUCT_DEFINITION_SHAPE($,$,#36);
#2228=PRODUCT_DEFINITION_SHAPE($,$,#37);
#2229=PRODUCT_DEFINITION_SHAPE($,$,#38);
#2230=PRODUCT_DEFINITION_SHAPE($,$,#39);
#2231=PRODUCT_DEFINITION_SHAPE($,$,#40);
#2232=PRODUCT_DEFINITION_SHAPE($,$,#41);
#2233=PRODUCT_DEFINITION_SHAPE($,$,#42);
#2234=SHAPE_REPRESENTATION('',(#1323,#1449,#1450,#1451,#1452,#1453,#1454,
#1455,#1456),#2194);
#2235=SHAPE_REPRESENTATION('',(#1324),#2195);
#2236=SHAPE_REPRESENTATION('',(#1370),#2196);
#2237=SHAPE_REPRESENTATION('',(#1376),#2197);
#2238=SHAPE_REPRESENTATION('',(#1382),#2198);
#2239=SHAPE_REPRESENTATION('',(#1395),#2199);
#2240=SHAPE_REPRESENTATION('',(#1414),#2200);
#2241=SHAPE_REPRESENTATION('',(#1434),#2201);
#2242=SHAPE_REPRESENTATION('',(#1440),#2202);
#2243=PRODUCT_DEFINITION_CONTEXT('part definition',#2272,'design');
#2244=PRODUCT_DEFINITION('BR-051','BR-051',#2253,#2243);
#2245=PRODUCT_DEFINITION('Wheel','Wheel',#2254,#2243);
#2246=PRODUCT_DEFINITION('Pin_01','Pin_01',#2255,#2243);
#2247=PRODUCT_DEFINITION('Pin_02','Pin_02',#2256,#2243);
#2248=PRODUCT_DEFINITION('Base','Base',#2257,#2243);
#2249=PRODUCT_DEFINITION('Crank_Bottom','Crank_Bottom',#2258,#2243);
#2250=PRODUCT_DEFINITION('Crank_Top','Crank_Top',#2259,#2243);
#2251=PRODUCT_DEFINITION('Pin_03','Pin_03',#2260,#2243);
#2252=PRODUCT_DEFINITION('Spacer','Spacer',#2261,#2243);
#2253=PRODUCT_DEFINITION_FORMATION('',$,#2274);
#2254=PRODUCT_DEFINITION_FORMATION('',$,#2275);
#2255=PRODUCT_DEFINITION_FORMATION('',$,#2276);
#2256=PRODUCT_DEFINITION_FORMATION('',$,#2277);
#2257=PRODUCT_DEFINITION_FORMATION('',$,#2278);
#2258=PRODUCT_DEFINITION_FORMATION('',$,#2279);
#2259=PRODUCT_DEFINITION_FORMATION('',$,#2280);
#2260=PRODUCT_DEFINITION_FORMATION('',$,#2281);
#2261=PRODUCT_DEFINITION_FORMATION('',$,#2282);
#2262=PRODUCT_RELATED_PRODUCT_CATEGORY('BR-051','BR-051',(#2274));
#2263=PRODUCT_RELATED_PRODUCT_CATEGORY('Wheel','Wheel',(#2275));
#2264=PRODUCT_RELATED_PRODUCT_CATEGORY('Pin_01','Pin_01',(#2276));
#2265=PRODUCT_RELATED_PRODUCT_CATEGORY('Pin_02','Pin_02',(#2277));
#2266=PRODUCT_RELATED_PRODUCT_CATEGORY('Base','Base',(#2278));
#2267=PRODUCT_RELATED_PRODUCT_CATEGORY('Crank_Bottom','Crank_Bottom',(#2279));
#2268=PRODUCT_RELATED_PRODUCT_CATEGORY('Crank_Top','Crank_Top',(#2280));
#2269=PRODUCT_RELATED_PRODUCT_CATEGORY('Pin_03','Pin_03',(#2281));
#2270=PRODUCT_RELATED_PRODUCT_CATEGORY('Spacer','Spacer',(#2282));
#2271=APPLICATION_PROTOCOL_DEFINITION('international standard',
'automotive_design',2009,#2272);
#2272=APPLICATION_CONTEXT(
'Core Data for Automotive Mechanical Design Process');
#2273=PRODUCT_CONTEXT('part definition',#2272,'mechanical');
#2274=PRODUCT('BR-051','BR-051',$,(#2273));
#2275=PRODUCT('Wheel','Wheel',$,(#2273));
#2276=PRODUCT('Pin_01','Pin_01',$,(#2273));
#2277=PRODUCT('Pin_02','Pin_02',$,(#2273));
#2278=PRODUCT('Base','Base',$,(#2273));
#2279=PRODUCT('Crank_Bottom','Crank_Bottom',$,(#2273));
#2280=PRODUCT('Crank_Top','Crank_Top',$,(#2273));
#2281=PRODUCT('Pin_03','Pin_03',$,(#2273));
#2282=PRODUCT('Spacer','Spacer',$,(#2273));
#2283=PRESENTATION_STYLE_ASSIGNMENT((#2287));
#2284=PRESENTATION_STYLE_ASSIGNMENT((#2288));
#2285=PRESENTATION_STYLE_ASSIGNMENT((#2289));
#2286=PRESENTATION_STYLE_ASSIGNMENT((#2290));
#2287=SURFACE_STYLE_USAGE(.BOTH.,#2291);
#2288=SURFACE_STYLE_USAGE(.BOTH.,#2292);
#2289=SURFACE_STYLE_USAGE(.BOTH.,#2293);
#2290=SURFACE_STYLE_USAGE(.BOTH.,#2294);
#2291=SURFACE_SIDE_STYLE('',(#2295));
#2292=SURFACE_SIDE_STYLE('',(#2296));
#2293=SURFACE_SIDE_STYLE('',(#2297));
#2294=SURFACE_SIDE_STYLE('',(#2298));
#2295=SURFACE_STYLE_FILL_AREA(#2299);
#2296=SURFACE_STYLE_FILL_AREA(#2300);
#2297=SURFACE_STYLE_FILL_AREA(#2301);
#2298=SURFACE_STYLE_FILL_AREA(#2302);
#2299=FILL_AREA_STYLE('Steel - Satin',(#2303));
#2300=FILL_AREA_STYLE('Surface - Matte',(#2304));
#2301=FILL_AREA_STYLE('Surface - Matte',(#2305));
#2302=FILL_AREA_STYLE('Surface - Matte',(#2306));
#2303=FILL_AREA_STYLE_COLOUR('Steel - Satin',#2307);
#2304=FILL_AREA_STYLE_COLOUR('Surface - Matte',#2308);
#2305=FILL_AREA_STYLE_COLOUR('Surface - Matte',#2309);
#2306=FILL_AREA_STYLE_COLOUR('Surface - Matte',#2310);
#2307=COLOUR_RGB('Steel - Satin', 0.09019608, 0.27058824, 0.51372549);
#2308=COLOUR_RGB('Surface - Matte', 0.09019608, 0.27058824, 0.51372549);
#2309=COLOUR_RGB('Surface - Matte', 0.66274510, 0.83137255, 0.94901961);
#2310=COLOUR_RGB('Surface - Matte', 0.31764706, 0.68627451, 0.89019608);
ENDSEC;
END-ISO-10303-21;
